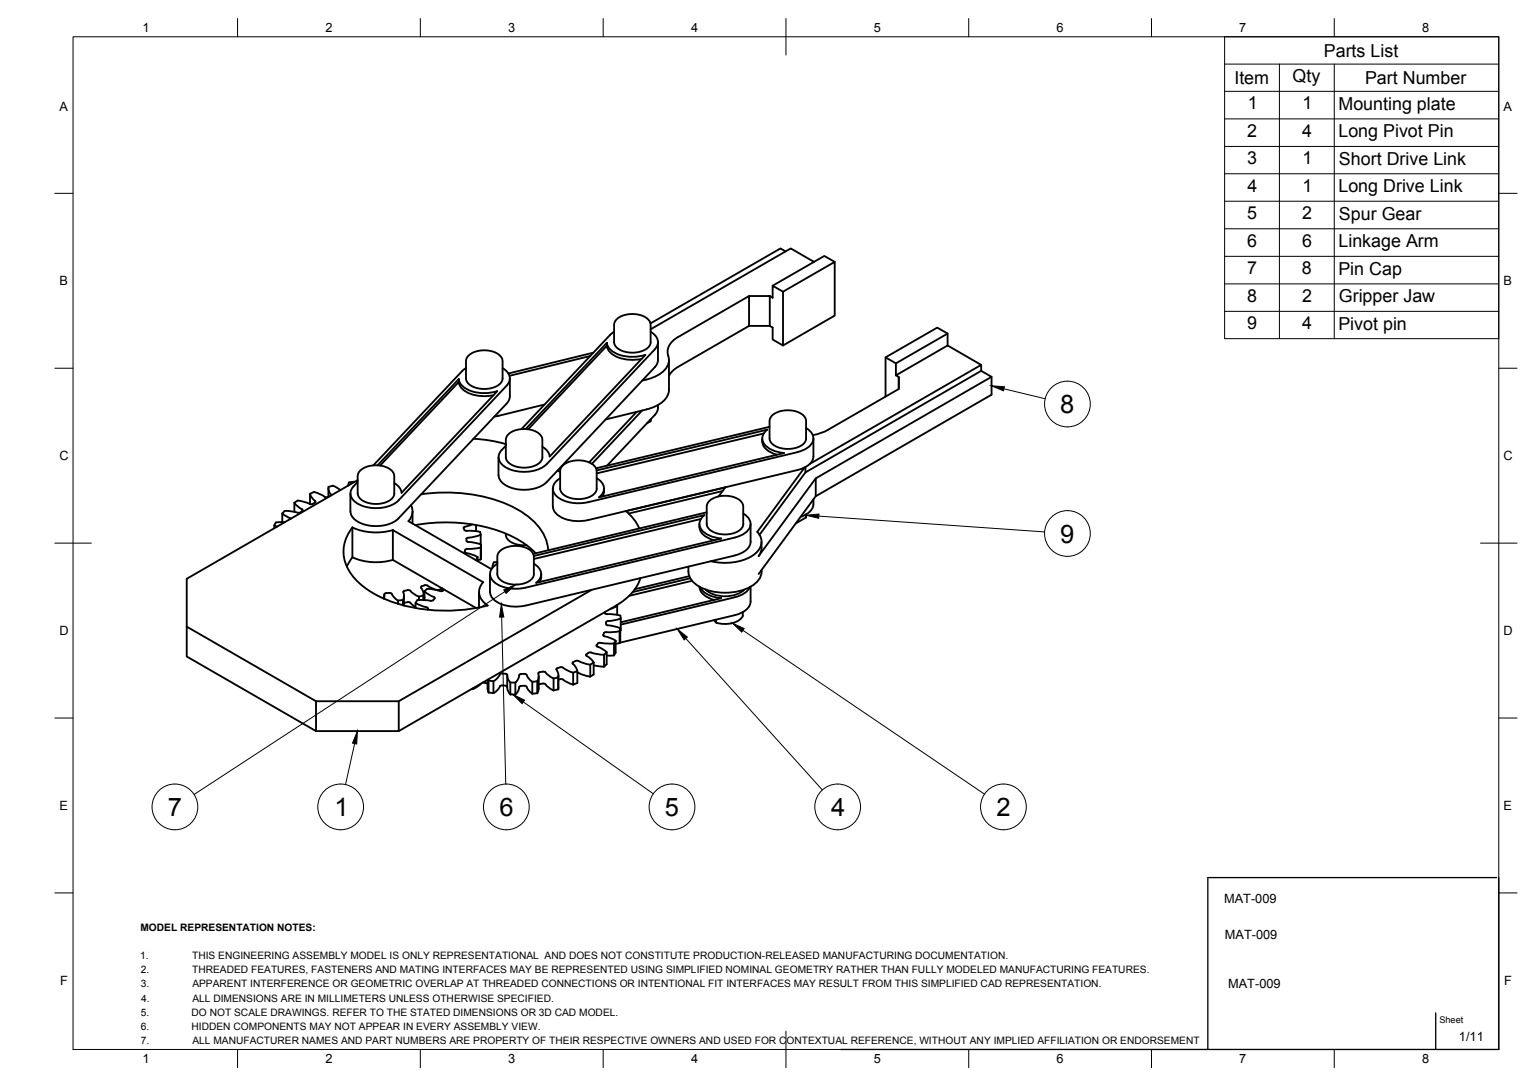
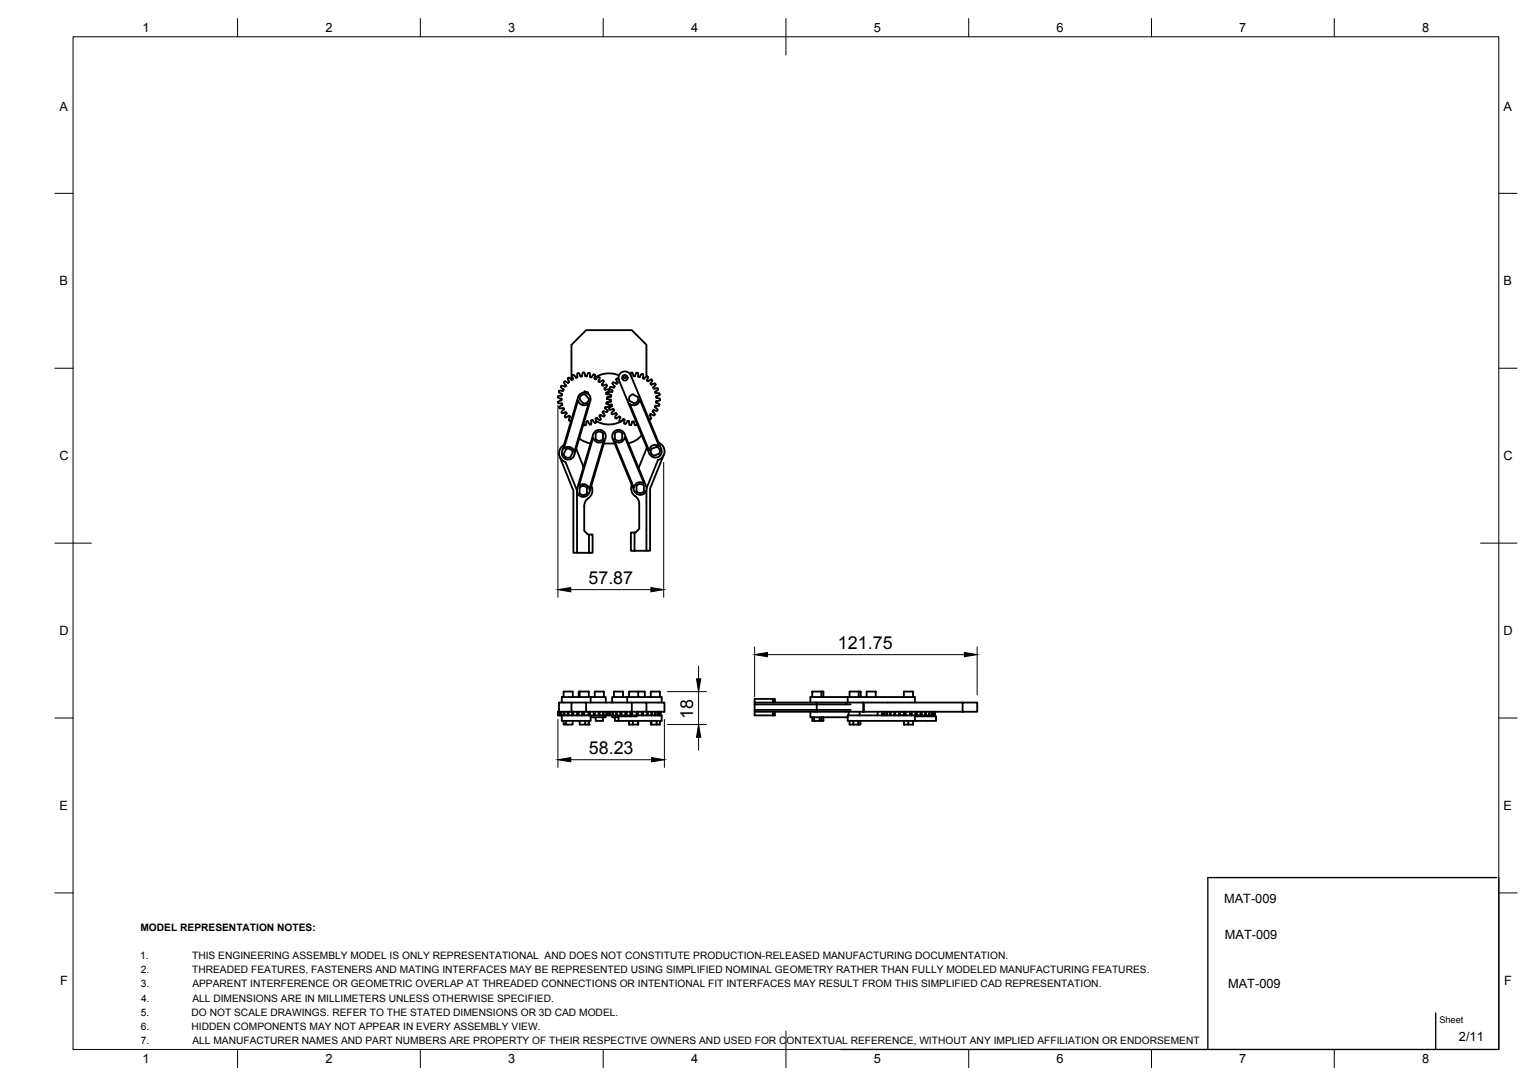
ISO-10303-21;
HEADER;
/* Generated by software containing ST-Developer
 * from STEP Tools, Inc. (www.steptools.com) 
 */

FILE_DESCRIPTION(
/* description */ ('STEP AP214'),
/* implementation_level */ '2;1');

FILE_NAME(
/* name */ 'MAT-009.step',
/* time_stamp */ '2026-11-14T05:43:09-08:00',
/* author */ (''),
/* organization */ (''),
/* preprocessor_version */ 'ST-DEVELOPER v20.2',
/* originating_system */ 'Autodesk Translation Framework v15.17.0.0',
/* authorisation */ '');

FILE_SCHEMA (('AUTOMOTIVE_DESIGN { 1 0 10303 214 3 1 1 }'));
ENDSEC;

DATA;
#10=MECHANICAL_DESIGN_GEOMETRIC_PRESENTATION_REPRESENTATION('',(#146,#147,
#148,#149,#150,#151,#152,#153,#154),#11933);
#11=ITEM_DEFINED_TRANSFORMATION($,$,#6753,#7621);
#12=ITEM_DEFINED_TRANSFORMATION($,$,#7486,#7622);
#13=ITEM_DEFINED_TRANSFORMATION($,$,#6800,#7623);
#14=ITEM_DEFINED_TRANSFORMATION($,$,#6849,#7624);
#15=ITEM_DEFINED_TRANSFORMATION($,$,#6899,#7625);
#16=ITEM_DEFINED_TRANSFORMATION($,$,#7521,#7626);
#17=ITEM_DEFINED_TRANSFORMATION($,$,#7591,#7627);
#18=ITEM_DEFINED_TRANSFORMATION($,$,#7448,#7628);
#19=ITEM_DEFINED_TRANSFORMATION($,$,#7556,#7629);
#20=ITEM_DEFINED_TRANSFORMATION($,$,#7486,#7630);
#21=ITEM_DEFINED_TRANSFORMATION($,$,#6899,#7631);
#22=ITEM_DEFINED_TRANSFORMATION($,$,#7521,#7632);
#23=ITEM_DEFINED_TRANSFORMATION($,$,#7591,#7633);
#24=ITEM_DEFINED_TRANSFORMATION($,$,#7448,#7634);
#25=ITEM_DEFINED_TRANSFORMATION($,$,#7486,#7635);
#26=ITEM_DEFINED_TRANSFORMATION($,$,#7486,#7636);
#27=ITEM_DEFINED_TRANSFORMATION($,$,#7591,#7637);
#28=ITEM_DEFINED_TRANSFORMATION($,$,#7591,#7638);
#29=ITEM_DEFINED_TRANSFORMATION($,$,#7521,#7639);
#30=ITEM_DEFINED_TRANSFORMATION($,$,#7521,#7640);
#31=ITEM_DEFINED_TRANSFORMATION($,$,#7521,#7641);
#32=ITEM_DEFINED_TRANSFORMATION($,$,#7521,#7642);
#33=ITEM_DEFINED_TRANSFORMATION($,$,#7556,#7643);
#34=ITEM_DEFINED_TRANSFORMATION($,$,#7556,#7644);
#35=ITEM_DEFINED_TRANSFORMATION($,$,#7556,#7645);
#36=ITEM_DEFINED_TRANSFORMATION($,$,#7591,#7646);
#37=ITEM_DEFINED_TRANSFORMATION($,$,#7591,#7647);
#38=ITEM_DEFINED_TRANSFORMATION($,$,#7591,#7648);
#39=ITEM_DEFINED_TRANSFORMATION($,$,#7591,#7649);
#40=(
REPRESENTATION_RELATIONSHIP($,$,#11988,#11987)
REPRESENTATION_RELATIONSHIP_WITH_TRANSFORMATION(#11)
SHAPE_REPRESENTATION_RELATIONSHIP()
);
#41=(
REPRESENTATION_RELATIONSHIP($,$,#11993,#11987)
REPRESENTATION_RELATIONSHIP_WITH_TRANSFORMATION(#12)
SHAPE_REPRESENTATION_RELATIONSHIP()
);
#42=(
REPRESENTATION_RELATIONSHIP($,$,#11989,#11987)
REPRESENTATION_RELATIONSHIP_WITH_TRANSFORMATION(#13)
SHAPE_REPRESENTATION_RELATIONSHIP()
);
#43=(
REPRESENTATION_RELATIONSHIP($,$,#11990,#11987)
REPRESENTATION_RELATIONSHIP_WITH_TRANSFORMATION(#14)
SHAPE_REPRESENTATION_RELATIONSHIP()
);
#44=(
REPRESENTATION_RELATIONSHIP($,$,#11991,#11987)
REPRESENTATION_RELATIONSHIP_WITH_TRANSFORMATION(#15)
SHAPE_REPRESENTATION_RELATIONSHIP()
);
#45=(
REPRESENTATION_RELATIONSHIP($,$,#11994,#11987)
REPRESENTATION_RELATIONSHIP_WITH_TRANSFORMATION(#16)
SHAPE_REPRESENTATION_RELATIONSHIP()
);
#46=(
REPRESENTATION_RELATIONSHIP($,$,#11996,#11987)
REPRESENTATION_RELATIONSHIP_WITH_TRANSFORMATION(#17)
SHAPE_REPRESENTATION_RELATIONSHIP()
);
#47=(
REPRESENTATION_RELATIONSHIP($,$,#11992,#11987)
REPRESENTATION_RELATIONSHIP_WITH_TRANSFORMATION(#18)
SHAPE_REPRESENTATION_RELATIONSHIP()
);
#48=(
REPRESENTATION_RELATIONSHIP($,$,#11995,#11987)
REPRESENTATION_RELATIONSHIP_WITH_TRANSFORMATION(#19)
SHAPE_REPRESENTATION_RELATIONSHIP()
);
#49=(
REPRESENTATION_RELATIONSHIP($,$,#11993,#11987)
REPRESENTATION_RELATIONSHIP_WITH_TRANSFORMATION(#20)
SHAPE_REPRESENTATION_RELATIONSHIP()
);
#50=(
REPRESENTATION_RELATIONSHIP($,$,#11991,#11987)
REPRESENTATION_RELATIONSHIP_WITH_TRANSFORMATION(#21)
SHAPE_REPRESENTATION_RELATIONSHIP()
);
#51=(
REPRESENTATION_RELATIONSHIP($,$,#11994,#11987)
REPRESENTATION_RELATIONSHIP_WITH_TRANSFORMATION(#22)
SHAPE_REPRESENTATION_RELATIONSHIP()
);
#52=(
REPRESENTATION_RELATIONSHIP($,$,#11996,#11987)
REPRESENTATION_RELATIONSHIP_WITH_TRANSFORMATION(#23)
SHAPE_REPRESENTATION_RELATIONSHIP()
);
#53=(
REPRESENTATION_RELATIONSHIP($,$,#11992,#11987)
REPRESENTATION_RELATIONSHIP_WITH_TRANSFORMATION(#24)
SHAPE_REPRESENTATION_RELATIONSHIP()
);
#54=(
REPRESENTATION_RELATIONSHIP($,$,#11993,#11987)
REPRESENTATION_RELATIONSHIP_WITH_TRANSFORMATION(#25)
SHAPE_REPRESENTATION_RELATIONSHIP()
);
#55=(
REPRESENTATION_RELATIONSHIP($,$,#11993,#11987)
REPRESENTATION_RELATIONSHIP_WITH_TRANSFORMATION(#26)
SHAPE_REPRESENTATION_RELATIONSHIP()
);
#56=(
REPRESENTATION_RELATIONSHIP($,$,#11996,#11987)
REPRESENTATION_RELATIONSHIP_WITH_TRANSFORMATION(#27)
SHAPE_REPRESENTATION_RELATIONSHIP()
);
#57=(
REPRESENTATION_RELATIONSHIP($,$,#11996,#11987)
REPRESENTATION_RELATIONSHIP_WITH_TRANSFORMATION(#28)
SHAPE_REPRESENTATION_RELATIONSHIP()
);
#58=(
REPRESENTATION_RELATIONSHIP($,$,#11994,#11987)
REPRESENTATION_RELATIONSHIP_WITH_TRANSFORMATION(#29)
SHAPE_REPRESENTATION_RELATIONSHIP()
);
#59=(
REPRESENTATION_RELATIONSHIP($,$,#11994,#11987)
REPRESENTATION_RELATIONSHIP_WITH_TRANSFORMATION(#30)
SHAPE_REPRESENTATION_RELATIONSHIP()
);
#60=(
REPRESENTATION_RELATIONSHIP($,$,#11994,#11987)
REPRESENTATION_RELATIONSHIP_WITH_TRANSFORMATION(#31)
SHAPE_REPRESENTATION_RELATIONSHIP()
);
#61=(
REPRESENTATION_RELATIONSHIP($,$,#11994,#11987)
REPRESENTATION_RELATIONSHIP_WITH_TRANSFORMATION(#32)
SHAPE_REPRESENTATION_RELATIONSHIP()
);
#62=(
REPRESENTATION_RELATIONSHIP($,$,#11995,#11987)
REPRESENTATION_RELATIONSHIP_WITH_TRANSFORMATION(#33)
SHAPE_REPRESENTATION_RELATIONSHIP()
);
#63=(
REPRESENTATION_RELATIONSHIP($,$,#11995,#11987)
REPRESENTATION_RELATIONSHIP_WITH_TRANSFORMATION(#34)
SHAPE_REPRESENTATION_RELATIONSHIP()
);
#64=(
REPRESENTATION_RELATIONSHIP($,$,#11995,#11987)
REPRESENTATION_RELATIONSHIP_WITH_TRANSFORMATION(#35)
SHAPE_REPRESENTATION_RELATIONSHIP()
);
#65=(
REPRESENTATION_RELATIONSHIP($,$,#11996,#11987)
REPRESENTATION_RELATIONSHIP_WITH_TRANSFORMATION(#36)
SHAPE_REPRESENTATION_RELATIONSHIP()
);
#66=(
REPRESENTATION_RELATIONSHIP($,$,#11996,#11987)
REPRESENTATION_RELATIONSHIP_WITH_TRANSFORMATION(#37)
SHAPE_REPRESENTATION_RELATIONSHIP()
);
#67=(
REPRESENTATION_RELATIONSHIP($,$,#11996,#11987)
REPRESENTATION_RELATIONSHIP_WITH_TRANSFORMATION(#38)
SHAPE_REPRESENTATION_RELATIONSHIP()
);
#68=(
REPRESENTATION_RELATIONSHIP($,$,#11996,#11987)
REPRESENTATION_RELATIONSHIP_WITH_TRANSFORMATION(#39)
SHAPE_REPRESENTATION_RELATIONSHIP()
);
#69=CONTEXT_DEPENDENT_SHAPE_REPRESENTATION(#40,#11958);
#70=CONTEXT_DEPENDENT_SHAPE_REPRESENTATION(#41,#11959);
#71=CONTEXT_DEPENDENT_SHAPE_REPRESENTATION(#42,#11960);
#72=CONTEXT_DEPENDENT_SHAPE_REPRESENTATION(#43,#11961);
#73=CONTEXT_DEPENDENT_SHAPE_REPRESENTATION(#44,#11962);
#74=CONTEXT_DEPENDENT_SHAPE_REPRESENTATION(#45,#11963);
#75=CONTEXT_DEPENDENT_SHAPE_REPRESENTATION(#46,#11964);
#76=CONTEXT_DEPENDENT_SHAPE_REPRESENTATION(#47,#11965);
#77=CONTEXT_DEPENDENT_SHAPE_REPRESENTATION(#48,#11966);
#78=CONTEXT_DEPENDENT_SHAPE_REPRESENTATION(#49,#11967);
#79=CONTEXT_DEPENDENT_SHAPE_REPRESENTATION(#50,#11968);
#80=CONTEXT_DEPENDENT_SHAPE_REPRESENTATION(#51,#11969);
#81=CONTEXT_DEPENDENT_SHAPE_REPRESENTATION(#52,#11970);
#82=CONTEXT_DEPENDENT_SHAPE_REPRESENTATION(#53,#11971);
#83=CONTEXT_DEPENDENT_SHAPE_REPRESENTATION(#54,#11972);
#84=CONTEXT_DEPENDENT_SHAPE_REPRESENTATION(#55,#11973);
#85=CONTEXT_DEPENDENT_SHAPE_REPRESENTATION(#56,#11974);
#86=CONTEXT_DEPENDENT_SHAPE_REPRESENTATION(#57,#11975);
#87=CONTEXT_DEPENDENT_SHAPE_REPRESENTATION(#58,#11976);
#88=CONTEXT_DEPENDENT_SHAPE_REPRESENTATION(#59,#11977);
#89=CONTEXT_DEPENDENT_SHAPE_REPRESENTATION(#60,#11978);
#90=CONTEXT_DEPENDENT_SHAPE_REPRESENTATION(#61,#11979);
#91=CONTEXT_DEPENDENT_SHAPE_REPRESENTATION(#62,#11980);
#92=CONTEXT_DEPENDENT_SHAPE_REPRESENTATION(#63,#11981);
#93=CONTEXT_DEPENDENT_SHAPE_REPRESENTATION(#64,#11982);
#94=CONTEXT_DEPENDENT_SHAPE_REPRESENTATION(#65,#11983);
#95=CONTEXT_DEPENDENT_SHAPE_REPRESENTATION(#66,#11984);
#96=CONTEXT_DEPENDENT_SHAPE_REPRESENTATION(#67,#11985);
#97=CONTEXT_DEPENDENT_SHAPE_REPRESENTATION(#68,#11986);
#98=NEXT_ASSEMBLY_USAGE_OCCURRENCE('Mounting Plate:1',
'Mounting Plate:1','Mounting Plate:1',#11998,#11999,'Mounting Plate:1');
#99=NEXT_ASSEMBLY_USAGE_OCCURRENCE('Long Pivot Pin:1',
'Long Pivot Pin:1','Long Pivot Pin:1',#11998,#12004,'Long Pivot Pin:1');
#100=NEXT_ASSEMBLY_USAGE_OCCURRENCE('Short Drive Link:1',
'Short Drive Link:1','Short Drive Link:1',#11998,#12000,
'Short Drive Link:1');
#101=NEXT_ASSEMBLY_USAGE_OCCURRENCE('Long Drive Link:1',
'Long Drive Link:1','Long Drive Link:1',#11998,#12001,
'Long Drive Link:1');
#102=NEXT_ASSEMBLY_USAGE_OCCURRENCE('Spur Gear:1','Spur Gear:1',
'Spur Gear:1',#11998,#12002,'Spur Gear:1');
#103=NEXT_ASSEMBLY_USAGE_OCCURRENCE('Linkage Arm:1','Linkage Arm:1',
'Linkage Arm:1',#11998,#12005,'Linkage Arm:1');
#104=NEXT_ASSEMBLY_USAGE_OCCURRENCE('Pin Cap:1','Pin Cap:1','Pin Cap:1',
#11998,#12007,'Pin Cap:1');
#105=NEXT_ASSEMBLY_USAGE_OCCURRENCE('Gripper Jaw:1','Gripper Jaw:1',
'Gripper Jaw:1',#11998,#12003,'Gripper Jaw:1');
#106=NEXT_ASSEMBLY_USAGE_OCCURRENCE('Pivot Pin:1','Pivot Pin:1',
'Pivot Pin:1',#11998,#12006,'Pivot Pin:1');
#107=NEXT_ASSEMBLY_USAGE_OCCURRENCE('Long Pivot Pin:2',
'Long Pivot Pin:2','Long Pivot Pin:2',#11998,#12004,'Long Pivot Pin:2');
#108=NEXT_ASSEMBLY_USAGE_OCCURRENCE('Spur Gear:2','Spur Gear:2',
'Spur Gear:2',#11998,#12002,'Spur Gear:2');
#109=NEXT_ASSEMBLY_USAGE_OCCURRENCE('Linkage Arm:2','Linkage Arm:2',
'Linkage Arm:2',#11998,#12005,'Linkage Arm:2');
#110=NEXT_ASSEMBLY_USAGE_OCCURRENCE('Pin Cap:2','Pin Cap:2','Pin Cap:2',
#11998,#12007,'Pin Cap:2');
#111=NEXT_ASSEMBLY_USAGE_OCCURRENCE('Gripper Jaw:2','Gripper Jaw:2',
'Gripper Jaw:2',#11998,#12003,'Gripper Jaw:2');
#112=NEXT_ASSEMBLY_USAGE_OCCURRENCE('Long Pivot Pin:3',
'Long Pivot Pin:3','Long Pivot Pin:3',#11998,#12004,'Long Pivot Pin:3');
#113=NEXT_ASSEMBLY_USAGE_OCCURRENCE('Long Pivot Pin:4',
'Long Pivot Pin:4','Long Pivot Pin:4',#11998,#12004,'Long Pivot Pin:4');
#114=NEXT_ASSEMBLY_USAGE_OCCURRENCE('Pin Cap:3','Pin Cap:3','Pin Cap:3',
#11998,#12007,'Pin Cap:3');
#115=NEXT_ASSEMBLY_USAGE_OCCURRENCE('Pin Cap:4','Pin Cap:4','Pin Cap:4',
#11998,#12007,'Pin Cap:4');
#116=NEXT_ASSEMBLY_USAGE_OCCURRENCE('Linkage Arm:3','Linkage Arm:3',
'Linkage Arm:3',#11998,#12005,'Linkage Arm:3');
#117=NEXT_ASSEMBLY_USAGE_OCCURRENCE('Linkage Arm:4','Linkage Arm:4',
'Linkage Arm:4',#11998,#12005,'Linkage Arm:4');
#118=NEXT_ASSEMBLY_USAGE_OCCURRENCE('Linkage Arm:5','Linkage Arm:5',
'Linkage Arm:5',#11998,#12005,'Linkage Arm:5');
#119=NEXT_ASSEMBLY_USAGE_OCCURRENCE('Linkage Arm:6','Linkage Arm:6',
'Linkage Arm:6',#11998,#12005,'Linkage Arm:6');
#120=NEXT_ASSEMBLY_USAGE_OCCURRENCE('Pivot Pin:2','Pivot Pin:2',
'Pivot Pin:2',#11998,#12006,'Pivot Pin:2');
#121=NEXT_ASSEMBLY_USAGE_OCCURRENCE('Pivot Pin:3','Pivot Pin:3',
'Pivot Pin:3',#11998,#12006,'Pivot Pin:3');
#122=NEXT_ASSEMBLY_USAGE_OCCURRENCE('Pivot Pin:4','Pivot Pin:4',
'Pivot Pin:4',#11998,#12006,'Pivot Pin:4');
#123=NEXT_ASSEMBLY_USAGE_OCCURRENCE('Pin Cap:5','Pin Cap:5','Pin Cap:5',
#11998,#12007,'Pin Cap:5');
#124=NEXT_ASSEMBLY_USAGE_OCCURRENCE('Pin Cap:6','Pin Cap:6','Pin Cap:6',
#11998,#12007,'Pin Cap:6');
#125=NEXT_ASSEMBLY_USAGE_OCCURRENCE('Pin Cap:7','Pin Cap:7','Pin Cap:7',
#11998,#12007,'Pin Cap:7');
#126=NEXT_ASSEMBLY_USAGE_OCCURRENCE('Pin Cap:8','Pin Cap:8','Pin Cap:8',
#11998,#12007,'Pin Cap:8');
#127=TOROIDAL_SURFACE('',#7592,2.4,0.1);
#128=SHAPE_REPRESENTATION_RELATIONSHIP('SRR','None',#11988,#137);
#129=SHAPE_REPRESENTATION_RELATIONSHIP('SRR','None',#11989,#138);
#130=SHAPE_REPRESENTATION_RELATIONSHIP('SRR','None',#11990,#139);
#131=SHAPE_REPRESENTATION_RELATIONSHIP('SRR','None',#11991,#140);
#132=SHAPE_REPRESENTATION_RELATIONSHIP('SRR','None',#11992,#141);
#133=SHAPE_REPRESENTATION_RELATIONSHIP('SRR','None',#11993,#142);
#134=SHAPE_REPRESENTATION_RELATIONSHIP('SRR','None',#11994,#143);
#135=SHAPE_REPRESENTATION_RELATIONSHIP('SRR','None',#11995,#144);
#136=SHAPE_REPRESENTATION_RELATIONSHIP('SRR','None',#11996,#145);
#137=ADVANCED_BREP_SHAPE_REPRESENTATION('',(#155),#11924);
#138=ADVANCED_BREP_SHAPE_REPRESENTATION('',(#156),#11925);
#139=ADVANCED_BREP_SHAPE_REPRESENTATION('',(#157),#11926);
#140=ADVANCED_BREP_SHAPE_REPRESENTATION('',(#158),#11927);
#141=ADVANCED_BREP_SHAPE_REPRESENTATION('',(#159),#11928);
#142=ADVANCED_BREP_SHAPE_REPRESENTATION('',(#160),#11929);
#143=ADVANCED_BREP_SHAPE_REPRESENTATION('',(#161),#11930);
#144=ADVANCED_BREP_SHAPE_REPRESENTATION('',(#162),#11931);
#145=ADVANCED_BREP_SHAPE_REPRESENTATION('',(#163),#11932);
#146=STYLED_ITEM('',(#12042),#155);
#147=STYLED_ITEM('',(#12042),#156);
#148=STYLED_ITEM('',(#12043),#157);
#149=STYLED_ITEM('',(#12043),#158);
#150=STYLED_ITEM('',(#12043),#159);
#151=STYLED_ITEM('',(#12042),#160);
#152=STYLED_ITEM('',(#12044),#161);
#153=STYLED_ITEM('',(#12043),#162);
#154=STYLED_ITEM('',(#12043),#163);
#155=MANIFOLD_SOLID_BREP('Body1',#6643);
#156=MANIFOLD_SOLID_BREP('Body1',#6644);
#157=MANIFOLD_SOLID_BREP('Body1',#6645);
#158=MANIFOLD_SOLID_BREP('Body1',#6646);
#159=MANIFOLD_SOLID_BREP('Body1',#6647);
#160=MANIFOLD_SOLID_BREP('Body1',#6648);
#161=MANIFOLD_SOLID_BREP('Body1',#6649);
#162=MANIFOLD_SOLID_BREP('Body1',#6650);
#163=MANIFOLD_SOLID_BREP('Body1',#6651);
#164=FACE_BOUND('',#692,.T.);
#165=FACE_BOUND('',#693,.T.);
#166=FACE_BOUND('',#694,.T.);
#167=FACE_BOUND('',#695,.T.);
#168=FACE_BOUND('',#696,.T.);
#169=FACE_BOUND('',#697,.T.);
#170=FACE_BOUND('',#699,.T.);
#171=FACE_BOUND('',#700,.T.);
#172=FACE_BOUND('',#701,.T.);
#173=FACE_BOUND('',#702,.T.);
#174=FACE_BOUND('',#703,.T.);
#175=FACE_BOUND('',#704,.T.);
#176=FACE_BOUND('',#714,.T.);
#177=FACE_BOUND('',#715,.T.);
#178=FACE_BOUND('',#717,.T.);
#179=FACE_BOUND('',#718,.T.);
#180=FACE_BOUND('',#719,.T.);
#181=FACE_BOUND('',#737,.T.);
#182=FACE_BOUND('',#739,.T.);
#183=FACE_BOUND('',#748,.T.);
#184=FACE_BOUND('',#750,.T.);
#185=FACE_BOUND('',#751,.T.);
#186=FACE_BOUND('',#753,.T.);
#187=FACE_BOUND('',#754,.T.);
#188=FACE_BOUND('',#755,.T.);
#189=FACE_BOUND('',#756,.T.);
#190=FACE_BOUND('',#773,.T.);
#191=FACE_BOUND('',#775,.T.);
#192=FACE_BOUND('',#825,.T.);
#193=FACE_BOUND('',#827,.T.);
#194=FACE_BOUND('',#968,.T.);
#195=FACE_BOUND('',#969,.T.);
#196=FACE_BOUND('',#972,.T.);
#197=FACE_BOUND('',#973,.T.);
#198=FACE_BOUND('',#998,.T.);
#199=FACE_BOUND('',#1000,.T.);
#200=FACE_BOUND('',#1019,.T.);
#201=FACE_BOUND('',#1020,.T.);
#202=FACE_BOUND('',#1021,.T.);
#203=FACE_BOUND('',#1026,.T.);
#204=FACE_BOUND('',#1027,.T.);
#205=FACE_BOUND('',#1028,.T.);
#206=FACE_BOUND('',#1042,.T.);
#207=FACE_BOUND('',#1051,.T.);
#208=FACE_BOUND('',#1064,.T.);
#209=PLANE('',#6766);
#210=PLANE('',#6767);
#211=PLANE('',#6768);
#212=PLANE('',#6769);
#213=PLANE('',#6770);
#214=PLANE('',#6777);
#215=PLANE('',#6787);
#216=PLANE('',#6791);
#217=PLANE('',#6792);
#218=PLANE('',#6795);
#219=PLANE('',#6821);
#220=PLANE('',#6825);
#221=PLANE('',#6828);
#222=PLANE('',#6830);
#223=PLANE('',#6833);
#224=PLANE('',#6834);
#225=PLANE('',#6835);
#226=PLANE('',#6836);
#227=PLANE('',#6839);
#228=PLANE('',#6840);
#229=PLANE('',#6841);
#230=PLANE('',#6842);
#231=PLANE('',#6845);
#232=PLANE('',#6846);
#233=PLANE('',#6847);
#234=PLANE('',#6848);
#235=PLANE('',#6871);
#236=PLANE('',#6872);
#237=PLANE('',#6876);
#238=PLANE('',#6879);
#239=PLANE('',#6881);
#240=PLANE('',#6884);
#241=PLANE('',#6885);
#242=PLANE('',#6886);
#243=PLANE('',#6887);
#244=PLANE('',#6890);
#245=PLANE('',#6891);
#246=PLANE('',#6892);
#247=PLANE('',#6895);
#248=PLANE('',#6896);
#249=PLANE('',#6897);
#250=PLANE('',#6898);
#251=PLANE('',#7044);
#252=PLANE('',#7178);
#253=PLANE('',#7445);
#254=PLANE('',#7446);
#255=PLANE('',#7447);
#256=PLANE('',#7460);
#257=PLANE('',#7463);
#258=PLANE('',#7464);
#259=PLANE('',#7467);
#260=PLANE('',#7468);
#261=PLANE('',#7469);
#262=PLANE('',#7470);
#263=PLANE('',#7471);
#264=PLANE('',#7473);
#265=PLANE('',#7474);
#266=PLANE('',#7475);
#267=PLANE('',#7476);
#268=PLANE('',#7477);
#269=PLANE('',#7478);
#270=PLANE('',#7479);
#271=PLANE('',#7480);
#272=PLANE('',#7481);
#273=PLANE('',#7482);
#274=PLANE('',#7483);
#275=PLANE('',#7484);
#276=PLANE('',#7497);
#277=PLANE('',#7501);
#278=PLANE('',#7502);
#279=PLANE('',#7507);
#280=PLANE('',#7510);
#281=PLANE('',#7511);
#282=PLANE('',#7512);
#283=PLANE('',#7516);
#284=PLANE('',#7517);
#285=PLANE('',#7518);
#286=PLANE('',#7519);
#287=PLANE('',#7520);
#288=PLANE('',#7537);
#289=PLANE('',#7540);
#290=PLANE('',#7541);
#291=PLANE('',#7544);
#292=PLANE('',#7546);
#293=PLANE('',#7549);
#294=PLANE('',#7550);
#295=PLANE('',#7553);
#296=PLANE('',#7554);
#297=PLANE('',#7555);
#298=PLANE('',#7567);
#299=PLANE('',#7571);
#300=PLANE('',#7572);
#301=PLANE('',#7576);
#302=PLANE('',#7577);
#303=PLANE('',#7578);
#304=PLANE('',#7579);
#305=PLANE('',#7580);
#306=PLANE('',#7581);
#307=PLANE('',#7586);
#308=PLANE('',#7589);
#309=PLANE('',#7590);
#310=PLANE('',#7609);
#311=PLANE('',#7611);
#312=PLANE('',#7612);
#313=PLANE('',#7615);
#314=PLANE('',#7616);
#315=PLANE('',#7617);
#316=PLANE('',#7618);
#317=PLANE('',#7619);
#318=PLANE('',#7620);
#319=FACE_OUTER_BOUND('',#673,.T.);
#320=FACE_OUTER_BOUND('',#674,.T.);
#321=FACE_OUTER_BOUND('',#675,.T.);
#322=FACE_OUTER_BOUND('',#676,.T.);
#323=FACE_OUTER_BOUND('',#677,.T.);
#324=FACE_OUTER_BOUND('',#678,.T.);
#325=FACE_OUTER_BOUND('',#679,.T.);
#326=FACE_OUTER_BOUND('',#680,.T.);
#327=FACE_OUTER_BOUND('',#681,.T.);
#328=FACE_OUTER_BOUND('',#682,.T.);
#329=FACE_OUTER_BOUND('',#683,.T.);
#330=FACE_OUTER_BOUND('',#684,.T.);
#331=FACE_OUTER_BOUND('',#685,.T.);
#332=FACE_OUTER_BOUND('',#686,.T.);
#333=FACE_OUTER_BOUND('',#687,.T.);
#334=FACE_OUTER_BOUND('',#688,.T.);
#335=FACE_OUTER_BOUND('',#689,.T.);
#336=FACE_OUTER_BOUND('',#690,.T.);
#337=FACE_OUTER_BOUND('',#691,.T.);
#338=FACE_OUTER_BOUND('',#698,.T.);
#339=FACE_OUTER_BOUND('',#705,.T.);
#340=FACE_OUTER_BOUND('',#706,.T.);
#341=FACE_OUTER_BOUND('',#707,.T.);
#342=FACE_OUTER_BOUND('',#708,.T.);
#343=FACE_OUTER_BOUND('',#709,.T.);
#344=FACE_OUTER_BOUND('',#710,.T.);
#345=FACE_OUTER_BOUND('',#711,.T.);
#346=FACE_OUTER_BOUND('',#712,.T.);
#347=FACE_OUTER_BOUND('',#713,.T.);
#348=FACE_OUTER_BOUND('',#716,.T.);
#349=FACE_OUTER_BOUND('',#720,.T.);
#350=FACE_OUTER_BOUND('',#721,.T.);
#351=FACE_OUTER_BOUND('',#722,.T.);
#352=FACE_OUTER_BOUND('',#723,.T.);
#353=FACE_OUTER_BOUND('',#724,.T.);
#354=FACE_OUTER_BOUND('',#725,.T.);
#355=FACE_OUTER_BOUND('',#726,.T.);
#356=FACE_OUTER_BOUND('',#727,.T.);
#357=FACE_OUTER_BOUND('',#728,.T.);
#358=FACE_OUTER_BOUND('',#729,.T.);
#359=FACE_OUTER_BOUND('',#730,.T.);
#360=FACE_OUTER_BOUND('',#731,.T.);
#361=FACE_OUTER_BOUND('',#732,.T.);
#362=FACE_OUTER_BOUND('',#733,.T.);
#363=FACE_OUTER_BOUND('',#734,.T.);
#364=FACE_OUTER_BOUND('',#735,.T.);
#365=FACE_OUTER_BOUND('',#736,.T.);
#366=FACE_OUTER_BOUND('',#738,.T.);
#367=FACE_OUTER_BOUND('',#740,.T.);
#368=FACE_OUTER_BOUND('',#741,.T.);
#369=FACE_OUTER_BOUND('',#742,.T.);
#370=FACE_OUTER_BOUND('',#743,.T.);
#371=FACE_OUTER_BOUND('',#744,.T.);
#372=FACE_OUTER_BOUND('',#745,.T.);
#373=FACE_OUTER_BOUND('',#746,.T.);
#374=FACE_OUTER_BOUND('',#747,.T.);
#375=FACE_OUTER_BOUND('',#749,.T.);
#376=FACE_OUTER_BOUND('',#752,.T.);
#377=FACE_OUTER_BOUND('',#757,.T.);
#378=FACE_OUTER_BOUND('',#758,.T.);
#379=FACE_OUTER_BOUND('',#759,.T.);
#380=FACE_OUTER_BOUND('',#760,.T.);
#381=FACE_OUTER_BOUND('',#761,.T.);
#382=FACE_OUTER_BOUND('',#762,.T.);
#383=FACE_OUTER_BOUND('',#763,.T.);
#384=FACE_OUTER_BOUND('',#764,.T.);
#385=FACE_OUTER_BOUND('',#765,.T.);
#386=FACE_OUTER_BOUND('',#766,.T.);
#387=FACE_OUTER_BOUND('',#767,.T.);
#388=FACE_OUTER_BOUND('',#768,.T.);
#389=FACE_OUTER_BOUND('',#769,.T.);
#390=FACE_OUTER_BOUND('',#770,.T.);
#391=FACE_OUTER_BOUND('',#771,.T.);
#392=FACE_OUTER_BOUND('',#772,.T.);
#393=FACE_OUTER_BOUND('',#774,.T.);
#394=FACE_OUTER_BOUND('',#776,.T.);
#395=FACE_OUTER_BOUND('',#777,.T.);
#396=FACE_OUTER_BOUND('',#778,.T.);
#397=FACE_OUTER_BOUND('',#779,.T.);
#398=FACE_OUTER_BOUND('',#780,.T.);
#399=FACE_OUTER_BOUND('',#781,.T.);
#400=FACE_OUTER_BOUND('',#782,.T.);
#401=FACE_OUTER_BOUND('',#783,.T.);
#402=FACE_OUTER_BOUND('',#784,.T.);
#403=FACE_OUTER_BOUND('',#785,.T.);
#404=FACE_OUTER_BOUND('',#786,.T.);
#405=FACE_OUTER_BOUND('',#787,.T.);
#406=FACE_OUTER_BOUND('',#788,.T.);
#407=FACE_OUTER_BOUND('',#789,.T.);
#408=FACE_OUTER_BOUND('',#790,.T.);
#409=FACE_OUTER_BOUND('',#791,.T.);
#410=FACE_OUTER_BOUND('',#792,.T.);
#411=FACE_OUTER_BOUND('',#793,.T.);
#412=FACE_OUTER_BOUND('',#794,.T.);
#413=FACE_OUTER_BOUND('',#795,.T.);
#414=FACE_OUTER_BOUND('',#796,.T.);
#415=FACE_OUTER_BOUND('',#797,.T.);
#416=FACE_OUTER_BOUND('',#798,.T.);
#417=FACE_OUTER_BOUND('',#799,.T.);
#418=FACE_OUTER_BOUND('',#800,.T.);
#419=FACE_OUTER_BOUND('',#801,.T.);
#420=FACE_OUTER_BOUND('',#802,.T.);
#421=FACE_OUTER_BOUND('',#803,.T.);
#422=FACE_OUTER_BOUND('',#804,.T.);
#423=FACE_OUTER_BOUND('',#805,.T.);
#424=FACE_OUTER_BOUND('',#806,.T.);
#425=FACE_OUTER_BOUND('',#807,.T.);
#426=FACE_OUTER_BOUND('',#808,.T.);
#427=FACE_OUTER_BOUND('',#809,.T.);
#428=FACE_OUTER_BOUND('',#810,.T.);
#429=FACE_OUTER_BOUND('',#811,.T.);
#430=FACE_OUTER_BOUND('',#812,.T.);
#431=FACE_OUTER_BOUND('',#813,.T.);
#432=FACE_OUTER_BOUND('',#814,.T.);
#433=FACE_OUTER_BOUND('',#815,.T.);
#434=FACE_OUTER_BOUND('',#816,.T.);
#435=FACE_OUTER_BOUND('',#817,.T.);
#436=FACE_OUTER_BOUND('',#818,.T.);
#437=FACE_OUTER_BOUND('',#819,.T.);
#438=FACE_OUTER_BOUND('',#820,.T.);
#439=FACE_OUTER_BOUND('',#821,.T.);
#440=FACE_OUTER_BOUND('',#822,.T.);
#441=FACE_OUTER_BOUND('',#823,.T.);
#442=FACE_OUTER_BOUND('',#824,.T.);
#443=FACE_OUTER_BOUND('',#826,.T.);
#444=FACE_OUTER_BOUND('',#828,.T.);
#445=FACE_OUTER_BOUND('',#829,.T.);
#446=FACE_OUTER_BOUND('',#830,.T.);
#447=FACE_OUTER_BOUND('',#831,.T.);
#448=FACE_OUTER_BOUND('',#832,.T.);
#449=FACE_OUTER_BOUND('',#833,.T.);
#450=FACE_OUTER_BOUND('',#834,.T.);
#451=FACE_OUTER_BOUND('',#835,.T.);
#452=FACE_OUTER_BOUND('',#836,.T.);
#453=FACE_OUTER_BOUND('',#837,.T.);
#454=FACE_OUTER_BOUND('',#838,.T.);
#455=FACE_OUTER_BOUND('',#839,.T.);
#456=FACE_OUTER_BOUND('',#840,.T.);
#457=FACE_OUTER_BOUND('',#841,.T.);
#458=FACE_OUTER_BOUND('',#842,.T.);
#459=FACE_OUTER_BOUND('',#843,.T.);
#460=FACE_OUTER_BOUND('',#844,.T.);
#461=FACE_OUTER_BOUND('',#845,.T.);
#462=FACE_OUTER_BOUND('',#846,.T.);
#463=FACE_OUTER_BOUND('',#847,.T.);
#464=FACE_OUTER_BOUND('',#848,.T.);
#465=FACE_OUTER_BOUND('',#849,.T.);
#466=FACE_OUTER_BOUND('',#850,.T.);
#467=FACE_OUTER_BOUND('',#851,.T.);
#468=FACE_OUTER_BOUND('',#852,.T.);
#469=FACE_OUTER_BOUND('',#853,.T.);
#470=FACE_OUTER_BOUND('',#854,.T.);
#471=FACE_OUTER_BOUND('',#855,.T.);
#472=FACE_OUTER_BOUND('',#856,.T.);
#473=FACE_OUTER_BOUND('',#857,.T.);
#474=FACE_OUTER_BOUND('',#858,.T.);
#475=FACE_OUTER_BOUND('',#859,.T.);
#476=FACE_OUTER_BOUND('',#860,.T.);
#477=FACE_OUTER_BOUND('',#861,.T.);
#478=FACE_OUTER_BOUND('',#862,.T.);
#479=FACE_OUTER_BOUND('',#863,.T.);
#480=FACE_OUTER_BOUND('',#864,.T.);
#481=FACE_OUTER_BOUND('',#865,.T.);
#482=FACE_OUTER_BOUND('',#866,.T.);
#483=FACE_OUTER_BOUND('',#867,.T.);
#484=FACE_OUTER_BOUND('',#868,.T.);
#485=FACE_OUTER_BOUND('',#869,.T.);
#486=FACE_OUTER_BOUND('',#870,.T.);
#487=FACE_OUTER_BOUND('',#871,.T.);
#488=FACE_OUTER_BOUND('',#872,.T.);
#489=FACE_OUTER_BOUND('',#873,.T.);
#490=FACE_OUTER_BOUND('',#874,.T.);
#491=FACE_OUTER_BOUND('',#875,.T.);
#492=FACE_OUTER_BOUND('',#876,.T.);
#493=FACE_OUTER_BOUND('',#877,.T.);
#494=FACE_OUTER_BOUND('',#878,.T.);
#495=FACE_OUTER_BOUND('',#879,.T.);
#496=FACE_OUTER_BOUND('',#880,.T.);
#497=FACE_OUTER_BOUND('',#881,.T.);
#498=FACE_OUTER_BOUND('',#882,.T.);
#499=FACE_OUTER_BOUND('',#883,.T.);
#500=FACE_OUTER_BOUND('',#884,.T.);
#501=FACE_OUTER_BOUND('',#885,.T.);
#502=FACE_OUTER_BOUND('',#886,.T.);
#503=FACE_OUTER_BOUND('',#887,.T.);
#504=FACE_OUTER_BOUND('',#888,.T.);
#505=FACE_OUTER_BOUND('',#889,.T.);
#506=FACE_OUTER_BOUND('',#890,.T.);
#507=FACE_OUTER_BOUND('',#891,.T.);
#508=FACE_OUTER_BOUND('',#892,.T.);
#509=FACE_OUTER_BOUND('',#893,.T.);
#510=FACE_OUTER_BOUND('',#894,.T.);
#511=FACE_OUTER_BOUND('',#895,.T.);
#512=FACE_OUTER_BOUND('',#896,.T.);
#513=FACE_OUTER_BOUND('',#897,.T.);
#514=FACE_OUTER_BOUND('',#898,.T.);
#515=FACE_OUTER_BOUND('',#899,.T.);
#516=FACE_OUTER_BOUND('',#900,.T.);
#517=FACE_OUTER_BOUND('',#901,.T.);
#518=FACE_OUTER_BOUND('',#902,.T.);
#519=FACE_OUTER_BOUND('',#903,.T.);
#520=FACE_OUTER_BOUND('',#904,.T.);
#521=FACE_OUTER_BOUND('',#905,.T.);
#522=FACE_OUTER_BOUND('',#906,.T.);
#523=FACE_OUTER_BOUND('',#907,.T.);
#524=FACE_OUTER_BOUND('',#908,.T.);
#525=FACE_OUTER_BOUND('',#909,.T.);
#526=FACE_OUTER_BOUND('',#910,.T.);
#527=FACE_OUTER_BOUND('',#911,.T.);
#528=FACE_OUTER_BOUND('',#912,.T.);
#529=FACE_OUTER_BOUND('',#913,.T.);
#530=FACE_OUTER_BOUND('',#914,.T.);
#531=FACE_OUTER_BOUND('',#915,.T.);
#532=FACE_OUTER_BOUND('',#916,.T.);
#533=FACE_OUTER_BOUND('',#917,.T.);
#534=FACE_OUTER_BOUND('',#918,.T.);
#535=FACE_OUTER_BOUND('',#919,.T.);
#536=FACE_OUTER_BOUND('',#920,.T.);
#537=FACE_OUTER_BOUND('',#921,.T.);
#538=FACE_OUTER_BOUND('',#922,.T.);
#539=FACE_OUTER_BOUND('',#923,.T.);
#540=FACE_OUTER_BOUND('',#924,.T.);
#541=FACE_OUTER_BOUND('',#925,.T.);
#542=FACE_OUTER_BOUND('',#926,.T.);
#543=FACE_OUTER_BOUND('',#927,.T.);
#544=FACE_OUTER_BOUND('',#928,.T.);
#545=FACE_OUTER_BOUND('',#929,.T.);
#546=FACE_OUTER_BOUND('',#930,.T.);
#547=FACE_OUTER_BOUND('',#931,.T.);
#548=FACE_OUTER_BOUND('',#932,.T.);
#549=FACE_OUTER_BOUND('',#933,.T.);
#550=FACE_OUTER_BOUND('',#934,.T.);
#551=FACE_OUTER_BOUND('',#935,.T.);
#552=FACE_OUTER_BOUND('',#936,.T.);
#553=FACE_OUTER_BOUND('',#937,.T.);
#554=FACE_OUTER_BOUND('',#938,.T.);
#555=FACE_OUTER_BOUND('',#939,.T.);
#556=FACE_OUTER_BOUND('',#940,.T.);
#557=FACE_OUTER_BOUND('',#941,.T.);
#558=FACE_OUTER_BOUND('',#942,.T.);
#559=FACE_OUTER_BOUND('',#943,.T.);
#560=FACE_OUTER_BOUND('',#944,.T.);
#561=FACE_OUTER_BOUND('',#945,.T.);
#562=FACE_OUTER_BOUND('',#946,.T.);
#563=FACE_OUTER_BOUND('',#947,.T.);
#564=FACE_OUTER_BOUND('',#948,.T.);
#565=FACE_OUTER_BOUND('',#949,.T.);
#566=FACE_OUTER_BOUND('',#950,.T.);
#567=FACE_OUTER_BOUND('',#951,.T.);
#568=FACE_OUTER_BOUND('',#952,.T.);
#569=FACE_OUTER_BOUND('',#953,.T.);
#570=FACE_OUTER_BOUND('',#954,.T.);
#571=FACE_OUTER_BOUND('',#955,.T.);
#572=FACE_OUTER_BOUND('',#956,.T.);
#573=FACE_OUTER_BOUND('',#957,.T.);
#574=FACE_OUTER_BOUND('',#958,.T.);
#575=FACE_OUTER_BOUND('',#959,.T.);
#576=FACE_OUTER_BOUND('',#960,.T.);
#577=FACE_OUTER_BOUND('',#961,.T.);
#578=FACE_OUTER_BOUND('',#962,.T.);
#579=FACE_OUTER_BOUND('',#963,.T.);
#580=FACE_OUTER_BOUND('',#964,.T.);
#581=FACE_OUTER_BOUND('',#965,.T.);
#582=FACE_OUTER_BOUND('',#966,.T.);
#583=FACE_OUTER_BOUND('',#967,.T.);
#584=FACE_OUTER_BOUND('',#970,.T.);
#585=FACE_OUTER_BOUND('',#971,.T.);
#586=FACE_OUTER_BOUND('',#974,.T.);
#587=FACE_OUTER_BOUND('',#975,.T.);
#588=FACE_OUTER_BOUND('',#976,.T.);
#589=FACE_OUTER_BOUND('',#977,.T.);
#590=FACE_OUTER_BOUND('',#978,.T.);
#591=FACE_OUTER_BOUND('',#979,.T.);
#592=FACE_OUTER_BOUND('',#980,.T.);
#593=FACE_OUTER_BOUND('',#981,.T.);
#594=FACE_OUTER_BOUND('',#982,.T.);
#595=FACE_OUTER_BOUND('',#983,.T.);
#596=FACE_OUTER_BOUND('',#984,.T.);
#597=FACE_OUTER_BOUND('',#985,.T.);
#598=FACE_OUTER_BOUND('',#986,.T.);
#599=FACE_OUTER_BOUND('',#987,.T.);
#600=FACE_OUTER_BOUND('',#988,.T.);
#601=FACE_OUTER_BOUND('',#989,.T.);
#602=FACE_OUTER_BOUND('',#990,.T.);
#603=FACE_OUTER_BOUND('',#991,.T.);
#604=FACE_OUTER_BOUND('',#992,.T.);
#605=FACE_OUTER_BOUND('',#993,.T.);
#606=FACE_OUTER_BOUND('',#994,.T.);
#607=FACE_OUTER_BOUND('',#995,.T.);
#608=FACE_OUTER_BOUND('',#996,.T.);
#609=FACE_OUTER_BOUND('',#997,.T.);
#610=FACE_OUTER_BOUND('',#999,.T.);
#611=FACE_OUTER_BOUND('',#1001,.T.);
#612=FACE_OUTER_BOUND('',#1002,.T.);
#613=FACE_OUTER_BOUND('',#1003,.T.);
#614=FACE_OUTER_BOUND('',#1004,.T.);
#615=FACE_OUTER_BOUND('',#1005,.T.);
#616=FACE_OUTER_BOUND('',#1006,.T.);
#617=FACE_OUTER_BOUND('',#1007,.T.);
#618=FACE_OUTER_BOUND('',#1008,.T.);
#619=FACE_OUTER_BOUND('',#1009,.T.);
#620=FACE_OUTER_BOUND('',#1010,.T.);
#621=FACE_OUTER_BOUND('',#1011,.T.);
#622=FACE_OUTER_BOUND('',#1012,.T.);
#623=FACE_OUTER_BOUND('',#1013,.T.);
#624=FACE_OUTER_BOUND('',#1014,.T.);
#625=FACE_OUTER_BOUND('',#1015,.T.);
#626=FACE_OUTER_BOUND('',#1016,.T.);
#627=FACE_OUTER_BOUND('',#1017,.T.);
#628=FACE_OUTER_BOUND('',#1018,.T.);
#629=FACE_OUTER_BOUND('',#1022,.T.);
#630=FACE_OUTER_BOUND('',#1023,.T.);
#631=FACE_OUTER_BOUND('',#1024,.T.);
#632=FACE_OUTER_BOUND('',#1025,.T.);
#633=FACE_OUTER_BOUND('',#1029,.T.);
#634=FACE_OUTER_BOUND('',#1030,.T.);
#635=FACE_OUTER_BOUND('',#1031,.T.);
#636=FACE_OUTER_BOUND('',#1032,.T.);
#637=FACE_OUTER_BOUND('',#1033,.T.);
#638=FACE_OUTER_BOUND('',#1034,.T.);
#639=FACE_OUTER_BOUND('',#1035,.T.);
#640=FACE_OUTER_BOUND('',#1036,.T.);
#641=FACE_OUTER_BOUND('',#1037,.T.);
#642=FACE_OUTER_BOUND('',#1038,.T.);
#643=FACE_OUTER_BOUND('',#1039,.T.);
#644=FACE_OUTER_BOUND('',#1040,.T.);
#645=FACE_OUTER_BOUND('',#1041,.T.);
#646=FACE_OUTER_BOUND('',#1043,.T.);
#647=FACE_OUTER_BOUND('',#1044,.T.);
#648=FACE_OUTER_BOUND('',#1045,.T.);
#649=FACE_OUTER_BOUND('',#1046,.T.);
#650=FACE_OUTER_BOUND('',#1047,.T.);
#651=FACE_OUTER_BOUND('',#1048,.T.);
#652=FACE_OUTER_BOUND('',#1049,.T.);
#653=FACE_OUTER_BOUND('',#1050,.T.);
#654=FACE_OUTER_BOUND('',#1052,.T.);
#655=FACE_OUTER_BOUND('',#1053,.T.);
#656=FACE_OUTER_BOUND('',#1054,.T.);
#657=FACE_OUTER_BOUND('',#1055,.T.);
#658=FACE_OUTER_BOUND('',#1056,.T.);
#659=FACE_OUTER_BOUND('',#1057,.T.);
#660=FACE_OUTER_BOUND('',#1058,.T.);
#661=FACE_OUTER_BOUND('',#1059,.T.);
#662=FACE_OUTER_BOUND('',#1060,.T.);
#663=FACE_OUTER_BOUND('',#1061,.T.);
#664=FACE_OUTER_BOUND('',#1062,.T.);
#665=FACE_OUTER_BOUND('',#1063,.T.);
#666=FACE_OUTER_BOUND('',#1065,.T.);
#667=FACE_OUTER_BOUND('',#1066,.T.);
#668=FACE_OUTER_BOUND('',#1067,.T.);
#669=FACE_OUTER_BOUND('',#1068,.T.);
#670=FACE_OUTER_BOUND('',#1069,.T.);
#671=FACE_OUTER_BOUND('',#1070,.T.);
#672=FACE_OUTER_BOUND('',#1071,.T.);
#673=EDGE_LOOP('',(#4112,#4113,#4114,#4115));
#674=EDGE_LOOP('',(#4116,#4117,#4118,#4119));
#675=EDGE_LOOP('',(#4120,#4121,#4122,#4123));
#676=EDGE_LOOP('',(#4124,#4125,#4126,#4127));
#677=EDGE_LOOP('',(#4128,#4129,#4130,#4131));
#678=EDGE_LOOP('',(#4132,#4133,#4134,#4135));
#679=EDGE_LOOP('',(#4136,#4137,#4138,#4139));
#680=EDGE_LOOP('',(#4140,#4141,#4142,#4143));
#681=EDGE_LOOP('',(#4144,#4145,#4146,#4147));
#682=EDGE_LOOP('',(#4148,#4149,#4150,#4151));
#683=EDGE_LOOP('',(#4152,#4153,#4154,#4155));
#684=EDGE_LOOP('',(#4156,#4157,#4158,#4159));
#685=EDGE_LOOP('',(#4160,#4161,#4162,#4163));
#686=EDGE_LOOP('',(#4164,#4165,#4166,#4167));
#687=EDGE_LOOP('',(#4168,#4169,#4170,#4171));
#688=EDGE_LOOP('',(#4172,#4173,#4174,#4175));
#689=EDGE_LOOP('',(#4176,#4177,#4178,#4179));
#690=EDGE_LOOP('',(#4180,#4181,#4182,#4183));
#691=EDGE_LOOP('',(#4184,#4185,#4186,#4187,#4188,#4189,#4190,#4191));
#692=EDGE_LOOP('',(#4192));
#693=EDGE_LOOP('',(#4193));
#694=EDGE_LOOP('',(#4194));
#695=EDGE_LOOP('',(#4195));
#696=EDGE_LOOP('',(#4196,#4197,#4198,#4199));
#697=EDGE_LOOP('',(#4200,#4201,#4202,#4203));
#698=EDGE_LOOP('',(#4204,#4205,#4206,#4207,#4208,#4209,#4210,#4211));
#699=EDGE_LOOP('',(#4212));
#700=EDGE_LOOP('',(#4213));
#701=EDGE_LOOP('',(#4214));
#702=EDGE_LOOP('',(#4215));
#703=EDGE_LOOP('',(#4216,#4217,#4218,#4219));
#704=EDGE_LOOP('',(#4220,#4221,#4222,#4223));
#705=EDGE_LOOP('',(#4224,#4225,#4226,#4227));
#706=EDGE_LOOP('',(#4228,#4229,#4230,#4231));
#707=EDGE_LOOP('',(#4232,#4233,#4234,#4235));
#708=EDGE_LOOP('',(#4236,#4237,#4238,#4239));
#709=EDGE_LOOP('',(#4240,#4241,#4242,#4243));
#710=EDGE_LOOP('',(#4244,#4245,#4246,#4247));
#711=EDGE_LOOP('',(#4248,#4249,#4250,#4251));
#712=EDGE_LOOP('',(#4252,#4253,#4254,#4255,#4256,#4257));
#713=EDGE_LOOP('',(#4258,#4259,#4260,#4261,#4262,#4263,#4264,#4265));
#714=EDGE_LOOP('',(#4266,#4267,#4268,#4269));
#715=EDGE_LOOP('',(#4270));
#716=EDGE_LOOP('',(#4271,#4272,#4273,#4274));
#717=EDGE_LOOP('',(#4275));
#718=EDGE_LOOP('',(#4276,#4277,#4278,#4279));
#719=EDGE_LOOP('',(#4280));
#720=EDGE_LOOP('',(#4281,#4282,#4283,#4284));
#721=EDGE_LOOP('',(#4285,#4286,#4287,#4288));
#722=EDGE_LOOP('',(#4289,#4290,#4291,#4292));
#723=EDGE_LOOP('',(#4293,#4294,#4295,#4296));
#724=EDGE_LOOP('',(#4297,#4298,#4299,#4300));
#725=EDGE_LOOP('',(#4301,#4302,#4303,#4304));
#726=EDGE_LOOP('',(#4305,#4306,#4307,#4308));
#727=EDGE_LOOP('',(#4309,#4310,#4311,#4312));
#728=EDGE_LOOP('',(#4313,#4314,#4315,#4316));
#729=EDGE_LOOP('',(#4317,#4318,#4319,#4320));
#730=EDGE_LOOP('',(#4321,#4322,#4323,#4324));
#731=EDGE_LOOP('',(#4325,#4326,#4327,#4328));
#732=EDGE_LOOP('',(#4329,#4330,#4331,#4332,#4333));
#733=EDGE_LOOP('',(#4334,#4335,#4336,#4337));
#734=EDGE_LOOP('',(#4338,#4339,#4340,#4341,#4342));
#735=EDGE_LOOP('',(#4343,#4344,#4345,#4346));
#736=EDGE_LOOP('',(#4347,#4348,#4349,#4350));
#737=EDGE_LOOP('',(#4351));
#738=EDGE_LOOP('',(#4352));
#739=EDGE_LOOP('',(#4353));
#740=EDGE_LOOP('',(#4354,#4355,#4356,#4357));
#741=EDGE_LOOP('',(#4358,#4359,#4360,#4361));
#742=EDGE_LOOP('',(#4362,#4363,#4364,#4365));
#743=EDGE_LOOP('',(#4366,#4367,#4368,#4369));
#744=EDGE_LOOP('',(#4370,#4371,#4372,#4373));
#745=EDGE_LOOP('',(#4374,#4375,#4376,#4377));
#746=EDGE_LOOP('',(#4378,#4379,#4380,#4381));
#747=EDGE_LOOP('',(#4382,#4383,#4384,#4385));
#748=EDGE_LOOP('',(#4386));
#749=EDGE_LOOP('',(#4387,#4388,#4389,#4390,#4391,#4392,#4393,#4394));
#750=EDGE_LOOP('',(#4395,#4396,#4397,#4398));
#751=EDGE_LOOP('',(#4399));
#752=EDGE_LOOP('',(#4400,#4401,#4402,#4403));
#753=EDGE_LOOP('',(#4404));
#754=EDGE_LOOP('',(#4405,#4406,#4407,#4408));
#755=EDGE_LOOP('',(#4409));
#756=EDGE_LOOP('',(#4410));
#757=EDGE_LOOP('',(#4411,#4412,#4413,#4414,#4415,#4416));
#758=EDGE_LOOP('',(#4417,#4418,#4419,#4420));
#759=EDGE_LOOP('',(#4421,#4422,#4423,#4424,#4425,#4426));
#760=EDGE_LOOP('',(#4427,#4428,#4429,#4430));
#761=EDGE_LOOP('',(#4431,#4432,#4433,#4434));
#762=EDGE_LOOP('',(#4435,#4436,#4437,#4438));
#763=EDGE_LOOP('',(#4439,#4440,#4441,#4442));
#764=EDGE_LOOP('',(#4443,#4444,#4445,#4446));
#765=EDGE_LOOP('',(#4447,#4448,#4449,#4450));
#766=EDGE_LOOP('',(#4451,#4452,#4453,#4454));
#767=EDGE_LOOP('',(#4455,#4456,#4457,#4458));
#768=EDGE_LOOP('',(#4459,#4460,#4461,#4462));
#769=EDGE_LOOP('',(#4463,#4464,#4465,#4466));
#770=EDGE_LOOP('',(#4467,#4468,#4469,#4470));
#771=EDGE_LOOP('',(#4471,#4472,#4473,#4474,#4475,#4476,#4477,#4478));
#772=EDGE_LOOP('',(#4479,#4480,#4481,#4482));
#773=EDGE_LOOP('',(#4483));
#774=EDGE_LOOP('',(#4484));
#775=EDGE_LOOP('',(#4485));
#776=EDGE_LOOP('',(#4486,#4487,#4488,#4489));
#777=EDGE_LOOP('',(#4490,#4491,#4492,#4493));
#778=EDGE_LOOP('',(#4494,#4495,#4496,#4497));
#779=EDGE_LOOP('',(#4498,#4499,#4500,#4501));
#780=EDGE_LOOP('',(#4502,#4503,#4504,#4505));
#781=EDGE_LOOP('',(#4506,#4507,#4508,#4509));
#782=EDGE_LOOP('',(#4510,#4511,#4512,#4513));
#783=EDGE_LOOP('',(#4514,#4515,#4516,#4517));
#784=EDGE_LOOP('',(#4518,#4519,#4520,#4521));
#785=EDGE_LOOP('',(#4522,#4523,#4524,#4525));
#786=EDGE_LOOP('',(#4526,#4527,#4528,#4529));
#787=EDGE_LOOP('',(#4530,#4531,#4532,#4533));
#788=EDGE_LOOP('',(#4534,#4535,#4536,#4537));
#789=EDGE_LOOP('',(#4538,#4539,#4540,#4541));
#790=EDGE_LOOP('',(#4542,#4543,#4544,#4545));
#791=EDGE_LOOP('',(#4546,#4547,#4548,#4549));
#792=EDGE_LOOP('',(#4550,#4551,#4552,#4553));
#793=EDGE_LOOP('',(#4554,#4555,#4556,#4557));
#794=EDGE_LOOP('',(#4558,#4559,#4560,#4561));
#795=EDGE_LOOP('',(#4562,#4563,#4564,#4565));
#796=EDGE_LOOP('',(#4566,#4567,#4568,#4569));
#797=EDGE_LOOP('',(#4570,#4571,#4572,#4573));
#798=EDGE_LOOP('',(#4574,#4575,#4576,#4577));
#799=EDGE_LOOP('',(#4578,#4579,#4580,#4581));
#800=EDGE_LOOP('',(#4582,#4583,#4584,#4585));
#801=EDGE_LOOP('',(#4586,#4587,#4588,#4589));
#802=EDGE_LOOP('',(#4590,#4591,#4592,#4593));
#803=EDGE_LOOP('',(#4594,#4595,#4596,#4597));
#804=EDGE_LOOP('',(#4598,#4599,#4600,#4601));
#805=EDGE_LOOP('',(#4602,#4603,#4604,#4605));
#806=EDGE_LOOP('',(#4606,#4607,#4608,#4609));
#807=EDGE_LOOP('',(#4610,#4611,#4612,#4613));
#808=EDGE_LOOP('',(#4614,#4615,#4616,#4617));
#809=EDGE_LOOP('',(#4618,#4619,#4620,#4621));
#810=EDGE_LOOP('',(#4622,#4623,#4624,#4625));
#811=EDGE_LOOP('',(#4626,#4627,#4628,#4629));
#812=EDGE_LOOP('',(#4630,#4631,#4632,#4633));
#813=EDGE_LOOP('',(#4634,#4635,#4636,#4637));
#814=EDGE_LOOP('',(#4638,#4639,#4640,#4641));
#815=EDGE_LOOP('',(#4642,#4643,#4644,#4645));
#816=EDGE_LOOP('',(#4646,#4647,#4648,#4649));
#817=EDGE_LOOP('',(#4650,#4651,#4652,#4653));
#818=EDGE_LOOP('',(#4654,#4655,#4656,#4657));
#819=EDGE_LOOP('',(#4658,#4659,#4660,#4661));
#820=EDGE_LOOP('',(#4662,#4663,#4664,#4665));
#821=EDGE_LOOP('',(#4666,#4667,#4668,#4669));
#822=EDGE_LOOP('',(#4670,#4671,#4672,#4673));
#823=EDGE_LOOP('',(#4674,#4675,#4676,#4677));
#824=EDGE_LOOP('',(#4678,#4679,#4680,#4681,#4682,#4683,#4684,#4685,#4686,
#4687,#4688,#4689,#4690,#4691,#4692,#4693,#4694,#4695,#4696,#4697,#4698,
#4699,#4700,#4701,#4702,#4703,#4704,#4705,#4706,#4707,#4708,#4709,#4710,
#4711,#4712,#4713,#4714,#4715,#4716,#4717,#4718,#4719,#4720,#4721,#4722,
#4723,#4724,#4725,#4726,#4727,#4728,#4729,#4730,#4731,#4732,#4733,#4734,
#4735,#4736,#4737,#4738,#4739,#4740,#4741,#4742,#4743,#4744,#4745,#4746,
#4747,#4748,#4749,#4750,#4751,#4752,#4753,#4754,#4755,#4756,#4757,#4758,
#4759,#4760,#4761,#4762,#4763,#4764,#4765,#4766,#4767,#4768,#4769,#4770,
#4771,#4772,#4773,#4774,#4775,#4776,#4777,#4778,#4779,#4780,#4781,#4782,
#4783,#4784,#4785,#4786,#4787,#4788,#4789,#4790,#4791,#4792,#4793,#4794,
#4795,#4796,#4797,#4798,#4799,#4800,#4801,#4802,#4803,#4804,#4805,#4806,
#4807,#4808,#4809,#4810,#4811,#4812,#4813,#4814,#4815,#4816,#4817,#4818,
#4819,#4820,#4821,#4822,#4823,#4824,#4825,#4826,#4827,#4828,#4829,#4830,
#4831,#4832,#4833,#4834,#4835,#4836,#4837,#4838,#4839,#4840,#4841,#4842,
#4843,#4844,#4845,#4846,#4847,#4848,#4849,#4850,#4851,#4852,#4853,#4854,
#4855,#4856,#4857));
#825=EDGE_LOOP('',(#4858,#4859,#4860,#4861));
#826=EDGE_LOOP('',(#4862,#4863,#4864,#4865,#4866,#4867,#4868,#4869,#4870,
#4871,#4872,#4873,#4874,#4875,#4876,#4877,#4878,#4879,#4880,#4881,#4882,
#4883,#4884,#4885,#4886,#4887,#4888,#4889,#4890,#4891,#4892,#4893,#4894,
#4895,#4896,#4897,#4898,#4899,#4900,#4901,#4902,#4903,#4904,#4905,#4906,
#4907,#4908,#4909,#4910,#4911,#4912,#4913,#4914,#4915,#4916,#4917,#4918,
#4919,#4920,#4921,#4922,#4923,#4924,#4925,#4926,#4927,#4928,#4929,#4930,
#4931,#4932,#4933,#4934,#4935,#4936,#4937,#4938,#4939,#4940,#4941,#4942,
#4943,#4944,#4945,#4946,#4947,#4948,#4949,#4950,#4951,#4952,#4953,#4954,
#4955,#4956,#4957,#4958,#4959,#4960,#4961,#4962,#4963,#4964,#4965,#4966,
#4967,#4968,#4969,#4970,#4971,#4972,#4973,#4974,#4975,#4976,#4977,#4978,
#4979,#4980,#4981,#4982,#4983,#4984,#4985,#4986,#4987,#4988,#4989,#4990,
#4991,#4992,#4993,#4994,#4995,#4996,#4997,#4998,#4999,#5000,#5001,#5002,
#5003,#5004,#5005,#5006,#5007,#5008,#5009,#5010,#5011,#5012,#5013,#5014,
#5015,#5016,#5017,#5018,#5019,#5020,#5021,#5022,#5023,#5024,#5025,#5026,
#5027,#5028,#5029,#5030,#5031,#5032,#5033,#5034,#5035,#5036,#5037,#5038,
#5039,#5040,#5041));
#827=EDGE_LOOP('',(#5042,#5043,#5044,#5045));
#828=EDGE_LOOP('',(#5046,#5047,#5048,#5049));
#829=EDGE_LOOP('',(#5050,#5051,#5052,#5053));
#830=EDGE_LOOP('',(#5054,#5055,#5056,#5057));
#831=EDGE_LOOP('',(#5058,#5059,#5060,#5061));
#832=EDGE_LOOP('',(#5062,#5063,#5064,#5065));
#833=EDGE_LOOP('',(#5066,#5067,#5068,#5069));
#834=EDGE_LOOP('',(#5070,#5071,#5072,#5073));
#835=EDGE_LOOP('',(#5074,#5075,#5076,#5077));
#836=EDGE_LOOP('',(#5078,#5079,#5080,#5081));
#837=EDGE_LOOP('',(#5082,#5083,#5084,#5085));
#838=EDGE_LOOP('',(#5086,#5087,#5088,#5089));
#839=EDGE_LOOP('',(#5090,#5091,#5092,#5093));
#840=EDGE_LOOP('',(#5094,#5095,#5096,#5097));
#841=EDGE_LOOP('',(#5098,#5099,#5100,#5101));
#842=EDGE_LOOP('',(#5102,#5103,#5104,#5105));
#843=EDGE_LOOP('',(#5106,#5107,#5108,#5109));
#844=EDGE_LOOP('',(#5110,#5111,#5112,#5113));
#845=EDGE_LOOP('',(#5114,#5115,#5116,#5117));
#846=EDGE_LOOP('',(#5118,#5119,#5120,#5121));
#847=EDGE_LOOP('',(#5122,#5123,#5124,#5125));
#848=EDGE_LOOP('',(#5126,#5127,#5128,#5129));
#849=EDGE_LOOP('',(#5130,#5131,#5132,#5133));
#850=EDGE_LOOP('',(#5134,#5135,#5136,#5137));
#851=EDGE_LOOP('',(#5138,#5139,#5140,#5141));
#852=EDGE_LOOP('',(#5142,#5143,#5144,#5145));
#853=EDGE_LOOP('',(#5146,#5147,#5148,#5149));
#854=EDGE_LOOP('',(#5150,#5151,#5152,#5153));
#855=EDGE_LOOP('',(#5154,#5155,#5156,#5157));
#856=EDGE_LOOP('',(#5158,#5159,#5160,#5161));
#857=EDGE_LOOP('',(#5162,#5163,#5164,#5165));
#858=EDGE_LOOP('',(#5166,#5167,#5168,#5169));
#859=EDGE_LOOP('',(#5170,#5171,#5172,#5173));
#860=EDGE_LOOP('',(#5174,#5175,#5176,#5177));
#861=EDGE_LOOP('',(#5178,#5179,#5180,#5181));
#862=EDGE_LOOP('',(#5182,#5183,#5184,#5185));
#863=EDGE_LOOP('',(#5186,#5187,#5188,#5189));
#864=EDGE_LOOP('',(#5190,#5191,#5192,#5193));
#865=EDGE_LOOP('',(#5194,#5195,#5196,#5197));
#866=EDGE_LOOP('',(#5198,#5199,#5200,#5201));
#867=EDGE_LOOP('',(#5202,#5203,#5204,#5205));
#868=EDGE_LOOP('',(#5206,#5207,#5208,#5209));
#869=EDGE_LOOP('',(#5210,#5211,#5212,#5213));
#870=EDGE_LOOP('',(#5214,#5215,#5216,#5217));
#871=EDGE_LOOP('',(#5218,#5219,#5220,#5221));
#872=EDGE_LOOP('',(#5222,#5223,#5224,#5225));
#873=EDGE_LOOP('',(#5226,#5227,#5228,#5229));
#874=EDGE_LOOP('',(#5230,#5231,#5232,#5233));
#875=EDGE_LOOP('',(#5234,#5235,#5236,#5237));
#876=EDGE_LOOP('',(#5238,#5239,#5240,#5241));
#877=EDGE_LOOP('',(#5242,#5243,#5244,#5245));
#878=EDGE_LOOP('',(#5246,#5247,#5248,#5249));
#879=EDGE_LOOP('',(#5250,#5251,#5252,#5253));
#880=EDGE_LOOP('',(#5254,#5255,#5256,#5257));
#881=EDGE_LOOP('',(#5258,#5259,#5260,#5261));
#882=EDGE_LOOP('',(#5262,#5263,#5264,#5265));
#883=EDGE_LOOP('',(#5266,#5267,#5268,#5269));
#884=EDGE_LOOP('',(#5270,#5271,#5272,#5273));
#885=EDGE_LOOP('',(#5274,#5275,#5276,#5277));
#886=EDGE_LOOP('',(#5278,#5279,#5280,#5281));
#887=EDGE_LOOP('',(#5282,#5283,#5284,#5285));
#888=EDGE_LOOP('',(#5286,#5287,#5288,#5289));
#889=EDGE_LOOP('',(#5290,#5291,#5292,#5293));
#890=EDGE_LOOP('',(#5294,#5295,#5296,#5297));
#891=EDGE_LOOP('',(#5298,#5299,#5300,#5301));
#892=EDGE_LOOP('',(#5302,#5303,#5304,#5305));
#893=EDGE_LOOP('',(#5306,#5307,#5308,#5309));
#894=EDGE_LOOP('',(#5310,#5311,#5312,#5313));
#895=EDGE_LOOP('',(#5314,#5315,#5316,#5317));
#896=EDGE_LOOP('',(#5318,#5319,#5320,#5321));
#897=EDGE_LOOP('',(#5322,#5323,#5324,#5325));
#898=EDGE_LOOP('',(#5326,#5327,#5328,#5329));
#899=EDGE_LOOP('',(#5330,#5331,#5332,#5333));
#900=EDGE_LOOP('',(#5334,#5335,#5336,#5337));
#901=EDGE_LOOP('',(#5338,#5339,#5340,#5341));
#902=EDGE_LOOP('',(#5342,#5343,#5344,#5345));
#903=EDGE_LOOP('',(#5346,#5347,#5348,#5349));
#904=EDGE_LOOP('',(#5350,#5351,#5352,#5353));
#905=EDGE_LOOP('',(#5354,#5355,#5356,#5357));
#906=EDGE_LOOP('',(#5358,#5359,#5360,#5361));
#907=EDGE_LOOP('',(#5362,#5363,#5364,#5365));
#908=EDGE_LOOP('',(#5366,#5367,#5368,#5369));
#909=EDGE_LOOP('',(#5370,#5371,#5372,#5373));
#910=EDGE_LOOP('',(#5374,#5375,#5376,#5377));
#911=EDGE_LOOP('',(#5378,#5379,#5380,#5381));
#912=EDGE_LOOP('',(#5382,#5383,#5384,#5385));
#913=EDGE_LOOP('',(#5386,#5387,#5388,#5389));
#914=EDGE_LOOP('',(#5390,#5391,#5392,#5393));
#915=EDGE_LOOP('',(#5394,#5395,#5396,#5397));
#916=EDGE_LOOP('',(#5398,#5399,#5400,#5401));
#917=EDGE_LOOP('',(#5402,#5403,#5404,#5405));
#918=EDGE_LOOP('',(#5406,#5407,#5408,#5409));
#919=EDGE_LOOP('',(#5410,#5411,#5412,#5413));
#920=EDGE_LOOP('',(#5414,#5415,#5416,#5417));
#921=EDGE_LOOP('',(#5418,#5419,#5420,#5421));
#922=EDGE_LOOP('',(#5422,#5423,#5424,#5425));
#923=EDGE_LOOP('',(#5426,#5427,#5428,#5429));
#924=EDGE_LOOP('',(#5430,#5431,#5432,#5433));
#925=EDGE_LOOP('',(#5434,#5435,#5436,#5437));
#926=EDGE_LOOP('',(#5438,#5439,#5440,#5441));
#927=EDGE_LOOP('',(#5442,#5443,#5444,#5445));
#928=EDGE_LOOP('',(#5446,#5447,#5448,#5449));
#929=EDGE_LOOP('',(#5450,#5451,#5452,#5453));
#930=EDGE_LOOP('',(#5454,#5455,#5456,#5457));
#931=EDGE_LOOP('',(#5458,#5459,#5460,#5461));
#932=EDGE_LOOP('',(#5462,#5463,#5464,#5465));
#933=EDGE_LOOP('',(#5466,#5467,#5468,#5469));
#934=EDGE_LOOP('',(#5470,#5471,#5472,#5473));
#935=EDGE_LOOP('',(#5474,#5475,#5476,#5477));
#936=EDGE_LOOP('',(#5478,#5479,#5480,#5481));
#937=EDGE_LOOP('',(#5482,#5483,#5484,#5485));
#938=EDGE_LOOP('',(#5486,#5487,#5488,#5489));
#939=EDGE_LOOP('',(#5490,#5491,#5492,#5493));
#940=EDGE_LOOP('',(#5494,#5495,#5496,#5497));
#941=EDGE_LOOP('',(#5498,#5499,#5500,#5501));
#942=EDGE_LOOP('',(#5502,#5503,#5504,#5505));
#943=EDGE_LOOP('',(#5506,#5507,#5508,#5509));
#944=EDGE_LOOP('',(#5510,#5511,#5512,#5513));
#945=EDGE_LOOP('',(#5514,#5515,#5516,#5517));
#946=EDGE_LOOP('',(#5518,#5519,#5520,#5521));
#947=EDGE_LOOP('',(#5522,#5523,#5524,#5525));
#948=EDGE_LOOP('',(#5526,#5527,#5528,#5529));
#949=EDGE_LOOP('',(#5530,#5531,#5532,#5533));
#950=EDGE_LOOP('',(#5534,#5535,#5536,#5537));
#951=EDGE_LOOP('',(#5538,#5539,#5540,#5541));
#952=EDGE_LOOP('',(#5542,#5543,#5544,#5545));
#953=EDGE_LOOP('',(#5546,#5547,#5548,#5549));
#954=EDGE_LOOP('',(#5550,#5551,#5552,#5553));
#955=EDGE_LOOP('',(#5554,#5555,#5556,#5557));
#956=EDGE_LOOP('',(#5558,#5559,#5560,#5561));
#957=EDGE_LOOP('',(#5562,#5563,#5564,#5565));
#958=EDGE_LOOP('',(#5566,#5567,#5568,#5569));
#959=EDGE_LOOP('',(#5570,#5571,#5572,#5573));
#960=EDGE_LOOP('',(#5574,#5575,#5576,#5577));
#961=EDGE_LOOP('',(#5578,#5579,#5580,#5581));
#962=EDGE_LOOP('',(#5582,#5583,#5584,#5585));
#963=EDGE_LOOP('',(#5586,#5587,#5588,#5589));
#964=EDGE_LOOP('',(#5590,#5591,#5592,#5593));
#965=EDGE_LOOP('',(#5594,#5595,#5596,#5597,#5598,#5599,#5600,#5601));
#966=EDGE_LOOP('',(#5602,#5603,#5604,#5605));
#967=EDGE_LOOP('',(#5606,#5607,#5608,#5609,#5610,#5611,#5612,#5613,#5614,
#5615,#5616));
#968=EDGE_LOOP('',(#5617));
#969=EDGE_LOOP('',(#5618));
#970=EDGE_LOOP('',(#5619,#5620,#5621,#5622,#5623,#5624));
#971=EDGE_LOOP('',(#5625,#5626,#5627,#5628,#5629,#5630,#5631,#5632,#5633,
#5634,#5635));
#972=EDGE_LOOP('',(#5636));
#973=EDGE_LOOP('',(#5637));
#974=EDGE_LOOP('',(#5638,#5639,#5640,#5641,#5642,#5643));
#975=EDGE_LOOP('',(#5644,#5645,#5646,#5647));
#976=EDGE_LOOP('',(#5648,#5649,#5650,#5651));
#977=EDGE_LOOP('',(#5652,#5653,#5654,#5655));
#978=EDGE_LOOP('',(#5656,#5657,#5658,#5659));
#979=EDGE_LOOP('',(#5660,#5661,#5662,#5663));
#980=EDGE_LOOP('',(#5664,#5665,#5666,#5667));
#981=EDGE_LOOP('',(#5668,#5669,#5670,#5671));
#982=EDGE_LOOP('',(#5672,#5673,#5674,#5675,#5676,#5677,#5678,#5679));
#983=EDGE_LOOP('',(#5680,#5681,#5682,#5683));
#984=EDGE_LOOP('',(#5684,#5685,#5686,#5687,#5688,#5689,#5690,#5691,#5692,
#5693,#5694,#5695));
#985=EDGE_LOOP('',(#5696,#5697,#5698,#5699));
#986=EDGE_LOOP('',(#5700,#5701,#5702,#5703));
#987=EDGE_LOOP('',(#5704,#5705,#5706,#5707));
#988=EDGE_LOOP('',(#5708,#5709,#5710,#5711));
#989=EDGE_LOOP('',(#5712,#5713,#5714,#5715));
#990=EDGE_LOOP('',(#5716,#5717,#5718,#5719));
#991=EDGE_LOOP('',(#5720,#5721,#5722,#5723));
#992=EDGE_LOOP('',(#5724,#5725,#5726,#5727));
#993=EDGE_LOOP('',(#5728,#5729,#5730,#5731,#5732,#5733,#5734,#5735,#5736,
#5737,#5738,#5739));
#994=EDGE_LOOP('',(#5740,#5741,#5742,#5743));
#995=EDGE_LOOP('',(#5744,#5745,#5746,#5747));
#996=EDGE_LOOP('',(#5748,#5749,#5750,#5751));
#997=EDGE_LOOP('',(#5752));
#998=EDGE_LOOP('',(#5753));
#999=EDGE_LOOP('',(#5754,#5755,#5756,#5757));
#1000=EDGE_LOOP('',(#5758));
#1001=EDGE_LOOP('',(#5759,#5760,#5761,#5762));
#1002=EDGE_LOOP('',(#5763,#5764,#5765,#5766));
#1003=EDGE_LOOP('',(#5767,#5768,#5769,#5770));
#1004=EDGE_LOOP('',(#5771,#5772,#5773,#5774));
#1005=EDGE_LOOP('',(#5775,#5776,#5777,#5778));
#1006=EDGE_LOOP('',(#5779,#5780,#5781,#5782,#5783));
#1007=EDGE_LOOP('',(#5784,#5785,#5786,#5787));
#1008=EDGE_LOOP('',(#5788,#5789,#5790,#5791,#5792,#5793,#5794,#5795));
#1009=EDGE_LOOP('',(#5796,#5797,#5798,#5799));
#1010=EDGE_LOOP('',(#5800,#5801,#5802,#5803));
#1011=EDGE_LOOP('',(#5804,#5805,#5806,#5807));
#1012=EDGE_LOOP('',(#5808,#5809,#5810,#5811));
#1013=EDGE_LOOP('',(#5812,#5813,#5814,#5815));
#1014=EDGE_LOOP('',(#5816,#5817,#5818,#5819));
#1015=EDGE_LOOP('',(#5820,#5821,#5822,#5823));
#1016=EDGE_LOOP('',(#5824,#5825,#5826,#5827));
#1017=EDGE_LOOP('',(#5828,#5829,#5830,#5831));
#1018=EDGE_LOOP('',(#5832,#5833,#5834,#5835));
#1019=EDGE_LOOP('',(#5836));
#1020=EDGE_LOOP('',(#5837));
#1021=EDGE_LOOP('',(#5838,#5839,#5840,#5841));
#1022=EDGE_LOOP('',(#5842,#5843,#5844,#5845));
#1023=EDGE_LOOP('',(#5846,#5847,#5848,#5849));
#1024=EDGE_LOOP('',(#5850,#5851,#5852,#5853));
#1025=EDGE_LOOP('',(#5854,#5855,#5856,#5857));
#1026=EDGE_LOOP('',(#5858,#5859,#5860,#5861));
#1027=EDGE_LOOP('',(#5862));
#1028=EDGE_LOOP('',(#5863));
#1029=EDGE_LOOP('',(#5864,#5865,#5866,#5867));
#1030=EDGE_LOOP('',(#5868,#5869,#5870,#5871));
#1031=EDGE_LOOP('',(#5872,#5873,#5874,#5875));
#1032=EDGE_LOOP('',(#5876,#5877,#5878,#5879));
#1033=EDGE_LOOP('',(#5880,#5881,#5882,#5883));
#1034=EDGE_LOOP('',(#5884,#5885,#5886,#5887));
#1035=EDGE_LOOP('',(#5888,#5889,#5890,#5891));
#1036=EDGE_LOOP('',(#5892,#5893,#5894,#5895));
#1037=EDGE_LOOP('',(#5896,#5897,#5898,#5899,#5900,#5901,#5902,#5903,#5904,
#5905,#5906,#5907));
#1038=EDGE_LOOP('',(#5908,#5909,#5910,#5911));
#1039=EDGE_LOOP('',(#5912,#5913,#5914,#5915));
#1040=EDGE_LOOP('',(#5916,#5917,#5918,#5919));
#1041=EDGE_LOOP('',(#5920));
#1042=EDGE_LOOP('',(#5921));
#1043=EDGE_LOOP('',(#5922,#5923,#5924,#5925,#5926));
#1044=EDGE_LOOP('',(#5927,#5928,#5929,#5930));
#1045=EDGE_LOOP('',(#5931,#5932,#5933,#5934,#5935,#5936,#5937,#5938));
#1046=EDGE_LOOP('',(#5939,#5940,#5941,#5942));
#1047=EDGE_LOOP('',(#5943,#5944,#5945,#5946));
#1048=EDGE_LOOP('',(#5947,#5948,#5949,#5950));
#1049=EDGE_LOOP('',(#5951,#5952,#5953,#5954));
#1050=EDGE_LOOP('',(#5955,#5956,#5957,#5958));
#1051=EDGE_LOOP('',(#5959));
#1052=EDGE_LOOP('',(#5960,#5961,#5962,#5963));
#1053=EDGE_LOOP('',(#5964,#5965,#5966,#5967));
#1054=EDGE_LOOP('',(#5968,#5969,#5970,#5971));
#1055=EDGE_LOOP('',(#5972,#5973,#5974,#5975));
#1056=EDGE_LOOP('',(#5976,#5977,#5978,#5979));
#1057=EDGE_LOOP('',(#5980,#5981,#5982,#5983,#5984));
#1058=EDGE_LOOP('',(#5985,#5986,#5987,#5988));
#1059=EDGE_LOOP('',(#5989,#5990,#5991,#5992,#5993));
#1060=EDGE_LOOP('',(#5994,#5995,#5996,#5997,#5998,#5999,#6000,#6001,#6002,
#6003,#6004,#6005));
#1061=EDGE_LOOP('',(#6006,#6007,#6008,#6009));
#1062=EDGE_LOOP('',(#6010,#6011,#6012,#6013));
#1063=EDGE_LOOP('',(#6014));
#1064=EDGE_LOOP('',(#6015,#6016,#6017,#6018,#6019,#6020,#6021,#6022,#6023));
#1065=EDGE_LOOP('',(#6024,#6025,#6026,#6027));
#1066=EDGE_LOOP('',(#6028,#6029,#6030,#6031));
#1067=EDGE_LOOP('',(#6032,#6033,#6034,#6035));
#1068=EDGE_LOOP('',(#6036,#6037,#6038,#6039));
#1069=EDGE_LOOP('',(#6040,#6041,#6042,#6043));
#1070=EDGE_LOOP('',(#6044));
#1071=EDGE_LOOP('',(#6045));
#1072=LINE('',#9914,#1534);
#1073=LINE('',#9920,#1535);
#1074=LINE('',#9926,#1536);
#1075=LINE('',#9932,#1537);
#1076=LINE('',#9937,#1538);
#1077=LINE('',#9939,#1539);
#1078=LINE('',#9941,#1540);
#1079=LINE('',#9942,#1541);
#1080=LINE('',#9945,#1542);
#1081=LINE('',#9947,#1543);
#1082=LINE('',#9948,#1544);
#1083=LINE('',#9951,#1545);
#1084=LINE('',#9953,#1546);
#1085=LINE('',#9954,#1547);
#1086=LINE('',#9957,#1548);
#1087=LINE('',#9959,#1549);
#1088=LINE('',#9960,#1550);
#1089=LINE('',#9964,#1551);
#1090=LINE('',#9966,#1552);
#1091=LINE('',#9968,#1553);
#1092=LINE('',#9969,#1554);
#1093=LINE('',#9975,#1555);
#1094=LINE('',#9978,#1556);
#1095=LINE('',#9983,#1557);
#1096=LINE('',#9987,#1558);
#1097=LINE('',#9989,#1559);
#1098=LINE('',#9990,#1560);
#1099=LINE('',#9996,#1561);
#1100=LINE('',#9999,#1562);
#1101=LINE('',#10004,#1563);
#1102=LINE('',#10010,#1564);
#1103=LINE('',#10014,#1565);
#1104=LINE('',#10016,#1566);
#1105=LINE('',#10017,#1567);
#1106=LINE('',#10022,#1568);
#1107=LINE('',#10023,#1569);
#1108=LINE('',#10037,#1570);
#1109=LINE('',#10044,#1571);
#1110=LINE('',#10047,#1572);
#1111=LINE('',#10053,#1573);
#1112=LINE('',#10056,#1574);
#1113=LINE('',#10061,#1575);
#1114=LINE('',#10067,#1576);
#1115=LINE('',#10076,#1577);
#1116=LINE('',#10080,#1578);
#1117=LINE('',#10086,#1579);
#1118=LINE('',#10088,#1580);
#1119=LINE('',#10091,#1581);
#1120=LINE('',#10092,#1582);
#1121=LINE('',#10096,#1583);
#1122=LINE('',#10097,#1584);
#1123=LINE('',#10100,#1585);
#1124=LINE('',#10103,#1586);
#1125=LINE('',#10105,#1587);
#1126=LINE('',#10108,#1588);
#1127=LINE('',#10110,#1589);
#1128=LINE('',#10112,#1590);
#1129=LINE('',#10116,#1591);
#1130=LINE('',#10119,#1592);
#1131=LINE('',#10121,#1593);
#1132=LINE('',#10123,#1594);
#1133=LINE('',#10127,#1595);
#1134=LINE('',#10128,#1596);
#1135=LINE('',#10132,#1597);
#1136=LINE('',#10134,#1598);
#1137=LINE('',#10138,#1599);
#1138=LINE('',#10140,#1600);
#1139=LINE('',#10141,#1601);
#1140=LINE('',#10144,#1602);
#1141=LINE('',#10146,#1603);
#1142=LINE('',#10147,#1604);
#1143=LINE('',#10150,#1605);
#1144=LINE('',#10154,#1606);
#1145=LINE('',#10155,#1607);
#1146=LINE('',#10157,#1608);
#1147=LINE('',#10165,#1609);
#1148=LINE('',#10172,#1610);
#1149=LINE('',#10175,#1611);
#1150=LINE('',#10180,#1612);
#1151=LINE('',#10187,#1613);
#1152=LINE('',#10190,#1614);
#1153=LINE('',#10196,#1615);
#1154=LINE('',#10199,#1616);
#1155=LINE('',#10204,#1617);
#1156=LINE('',#10210,#1618);
#1157=LINE('',#10214,#1619);
#1158=LINE('',#10216,#1620);
#1159=LINE('',#10217,#1621);
#1160=LINE('',#10223,#1622);
#1161=LINE('',#10225,#1623);
#1162=LINE('',#10227,#1624);
#1163=LINE('',#10231,#1625);
#1164=LINE('',#10233,#1626);
#1165=LINE('',#10234,#1627);
#1166=LINE('',#10238,#1628);
#1167=LINE('',#10239,#1629);
#1168=LINE('',#10242,#1630);
#1169=LINE('',#10244,#1631);
#1170=LINE('',#10247,#1632);
#1171=LINE('',#10250,#1633);
#1172=LINE('',#10252,#1634);
#1173=LINE('',#10253,#1635);
#1174=LINE('',#10255,#1636);
#1175=LINE('',#10257,#1637);
#1176=LINE('',#10260,#1638);
#1177=LINE('',#10263,#1639);
#1178=LINE('',#10265,#1640);
#1179=LINE('',#10267,#1641);
#1180=LINE('',#10271,#1642);
#1181=LINE('',#10272,#1643);
#1182=LINE('',#10276,#1644);
#1183=LINE('',#10278,#1645);
#1184=LINE('',#10282,#1646);
#1185=LINE('',#10284,#1647);
#1186=LINE('',#10285,#1648);
#1187=LINE('',#10288,#1649);
#1188=LINE('',#10292,#1650);
#1189=LINE('',#10293,#1651);
#1190=LINE('',#10295,#1652);
#1191=LINE('',#10304,#1653);
#1192=LINE('',#10307,#1654);
#1193=LINE('',#10313,#1655);
#1194=LINE('',#10316,#1656);
#1195=LINE('',#10321,#1657);
#1196=LINE('',#10328,#1658);
#1197=LINE('',#10331,#1659);
#1198=LINE('',#10336,#1660);
#1199=LINE('',#10343,#1661);
#1200=LINE('',#10346,#1662);
#1201=LINE('',#10352,#1663);
#1202=LINE('',#10358,#1664);
#1203=LINE('',#10361,#1665);
#1204=LINE('',#10367,#1666);
#1205=LINE('',#10373,#1667);
#1206=LINE('',#10376,#1668);
#1207=LINE('',#10382,#1669);
#1208=LINE('',#10385,#1670);
#1209=LINE('',#10391,#1671);
#1210=LINE('',#10394,#1672);
#1211=LINE('',#10400,#1673);
#1212=LINE('',#10403,#1674);
#1213=LINE('',#10409,#1675);
#1214=LINE('',#10412,#1676);
#1215=LINE('',#10418,#1677);
#1216=LINE('',#10421,#1678);
#1217=LINE('',#10427,#1679);
#1218=LINE('',#10430,#1680);
#1219=LINE('',#10436,#1681);
#1220=LINE('',#10439,#1682);
#1221=LINE('',#10445,#1683);
#1222=LINE('',#10448,#1684);
#1223=LINE('',#10454,#1685);
#1224=LINE('',#10457,#1686);
#1225=LINE('',#10463,#1687);
#1226=LINE('',#10466,#1688);
#1227=LINE('',#10472,#1689);
#1228=LINE('',#10475,#1690);
#1229=LINE('',#10481,#1691);
#1230=LINE('',#10484,#1692);
#1231=LINE('',#10490,#1693);
#1232=LINE('',#10493,#1694);
#1233=LINE('',#10499,#1695);
#1234=LINE('',#10502,#1696);
#1235=LINE('',#10508,#1697);
#1236=LINE('',#10511,#1698);
#1237=LINE('',#10517,#1699);
#1238=LINE('',#10520,#1700);
#1239=LINE('',#10526,#1701);
#1240=LINE('',#10529,#1702);
#1241=LINE('',#10535,#1703);
#1242=LINE('',#10538,#1704);
#1243=LINE('',#10544,#1705);
#1244=LINE('',#10547,#1706);
#1245=LINE('',#10553,#1707);
#1246=LINE('',#10556,#1708);
#1247=LINE('',#10562,#1709);
#1248=LINE('',#10565,#1710);
#1249=LINE('',#10571,#1711);
#1250=LINE('',#10574,#1712);
#1251=LINE('',#10580,#1713);
#1252=LINE('',#10583,#1714);
#1253=LINE('',#10588,#1715);
#1254=LINE('',#10594,#1716);
#1255=LINE('',#10600,#1717);
#1256=LINE('',#10607,#1718);
#1257=LINE('',#10610,#1719);
#1258=LINE('',#10616,#1720);
#1259=LINE('',#10619,#1721);
#1260=LINE('',#10625,#1722);
#1261=LINE('',#10628,#1723);
#1262=LINE('',#10634,#1724);
#1263=LINE('',#10637,#1725);
#1264=LINE('',#10643,#1726);
#1265=LINE('',#10646,#1727);
#1266=LINE('',#10652,#1728);
#1267=LINE('',#10655,#1729);
#1268=LINE('',#10661,#1730);
#1269=LINE('',#10664,#1731);
#1270=LINE('',#10670,#1732);
#1271=LINE('',#10673,#1733);
#1272=LINE('',#10679,#1734);
#1273=LINE('',#10682,#1735);
#1274=LINE('',#10688,#1736);
#1275=LINE('',#10691,#1737);
#1276=LINE('',#10697,#1738);
#1277=LINE('',#10700,#1739);
#1278=LINE('',#10706,#1740);
#1279=LINE('',#10709,#1741);
#1280=LINE('',#10938,#1742);
#1281=LINE('',#10940,#1743);
#1282=LINE('',#10941,#1744);
#1283=LINE('',#11170,#1745);
#1284=LINE('',#11172,#1746);
#1285=LINE('',#11173,#1747);
#1286=LINE('',#11175,#1748);
#1287=LINE('',#11177,#1749);
#1288=LINE('',#11179,#1750);
#1289=LINE('',#11181,#1751);
#1290=LINE('',#11182,#1752);
#1291=LINE('',#11186,#1753);
#1292=LINE('',#11188,#1754);
#1293=LINE('',#11190,#1755);
#1294=LINE('',#11192,#1756);
#1295=LINE('',#11196,#1757);
#1296=LINE('',#11198,#1758);
#1297=LINE('',#11202,#1759);
#1298=LINE('',#11204,#1760);
#1299=LINE('',#11208,#1761);
#1300=LINE('',#11210,#1762);
#1301=LINE('',#11214,#1763);
#1302=LINE('',#11216,#1764);
#1303=LINE('',#11220,#1765);
#1304=LINE('',#11222,#1766);
#1305=LINE('',#11225,#1767);
#1306=LINE('',#11228,#1768);
#1307=LINE('',#11231,#1769);
#1308=LINE('',#11234,#1770);
#1309=LINE('',#11237,#1771);
#1310=LINE('',#11240,#1772);
#1311=LINE('',#11243,#1773);
#1312=LINE('',#11246,#1774);
#1313=LINE('',#11249,#1775);
#1314=LINE('',#11252,#1776);
#1315=LINE('',#11255,#1777);
#1316=LINE('',#11257,#1778);
#1317=LINE('',#11260,#1779);
#1318=LINE('',#11262,#1780);
#1319=LINE('',#11265,#1781);
#1320=LINE('',#11267,#1782);
#1321=LINE('',#11270,#1783);
#1322=LINE('',#11272,#1784);
#1323=LINE('',#11275,#1785);
#1324=LINE('',#11277,#1786);
#1325=LINE('',#11279,#1787);
#1326=LINE('',#11281,#1788);
#1327=LINE('',#11284,#1789);
#1328=LINE('',#11286,#1790);
#1329=LINE('',#11288,#1791);
#1330=LINE('',#11290,#1792);
#1331=LINE('',#11293,#1793);
#1332=LINE('',#11295,#1794);
#1333=LINE('',#11297,#1795);
#1334=LINE('',#11299,#1796);
#1335=LINE('',#11302,#1797);
#1336=LINE('',#11304,#1798);
#1337=LINE('',#11306,#1799);
#1338=LINE('',#11308,#1800);
#1339=LINE('',#11311,#1801);
#1340=LINE('',#11313,#1802);
#1341=LINE('',#11315,#1803);
#1342=LINE('',#11317,#1804);
#1343=LINE('',#11320,#1805);
#1344=LINE('',#11322,#1806);
#1345=LINE('',#11324,#1807);
#1346=LINE('',#11326,#1808);
#1347=LINE('',#11329,#1809);
#1348=LINE('',#11331,#1810);
#1349=LINE('',#11333,#1811);
#1350=LINE('',#11335,#1812);
#1351=LINE('',#11338,#1813);
#1352=LINE('',#11340,#1814);
#1353=LINE('',#11342,#1815);
#1354=LINE('',#11344,#1816);
#1355=LINE('',#11347,#1817);
#1356=LINE('',#11349,#1818);
#1357=LINE('',#11351,#1819);
#1358=LINE('',#11353,#1820);
#1359=LINE('',#11356,#1821);
#1360=LINE('',#11358,#1822);
#1361=LINE('',#11360,#1823);
#1362=LINE('',#11362,#1824);
#1363=LINE('',#11365,#1825);
#1364=LINE('',#11367,#1826);
#1365=LINE('',#11369,#1827);
#1366=LINE('',#11371,#1828);
#1367=LINE('',#11374,#1829);
#1368=LINE('',#11376,#1830);
#1369=LINE('',#11378,#1831);
#1370=LINE('',#11380,#1832);
#1371=LINE('',#11383,#1833);
#1372=LINE('',#11385,#1834);
#1373=LINE('',#11387,#1835);
#1374=LINE('',#11389,#1836);
#1375=LINE('',#11392,#1837);
#1376=LINE('',#11394,#1838);
#1377=LINE('',#11396,#1839);
#1378=LINE('',#11398,#1840);
#1379=LINE('',#11401,#1841);
#1380=LINE('',#11403,#1842);
#1381=LINE('',#11410,#1843);
#1382=LINE('',#11417,#1844);
#1383=LINE('',#11421,#1845);
#1384=LINE('',#11425,#1846);
#1385=LINE('',#11428,#1847);
#1386=LINE('',#11433,#1848);
#1387=LINE('',#11438,#1849);
#1388=LINE('',#11440,#1850);
#1389=LINE('',#11442,#1851);
#1390=LINE('',#11444,#1852);
#1391=LINE('',#11445,#1853);
#1392=LINE('',#11447,#1854);
#1393=LINE('',#11453,#1855);
#1394=LINE('',#11454,#1856);
#1395=LINE('',#11457,#1857);
#1396=LINE('',#11459,#1858);
#1397=LINE('',#11461,#1859);
#1398=LINE('',#11463,#1860);
#1399=LINE('',#11464,#1861);
#1400=LINE('',#11468,#1862);
#1401=LINE('',#11470,#1863);
#1402=LINE('',#11472,#1864);
#1403=LINE('',#11474,#1865);
#1404=LINE('',#11479,#1866);
#1405=LINE('',#11481,#1867);
#1406=LINE('',#11483,#1868);
#1407=LINE('',#11484,#1869);
#1408=LINE('',#11488,#1870);
#1409=LINE('',#11489,#1871);
#1410=LINE('',#11491,#1872);
#1411=LINE('',#11493,#1873);
#1412=LINE('',#11494,#1874);
#1413=LINE('',#11496,#1875);
#1414=LINE('',#11498,#1876);
#1415=LINE('',#11500,#1877);
#1416=LINE('',#11502,#1878);
#1417=LINE('',#11504,#1879);
#1418=LINE('',#11506,#1880);
#1419=LINE('',#11507,#1881);
#1420=LINE('',#11509,#1882);
#1421=LINE('',#11512,#1883);
#1422=LINE('',#11514,#1884);
#1423=LINE('',#11516,#1885);
#1424=LINE('',#11518,#1886);
#1425=LINE('',#11519,#1887);
#1426=LINE('',#11522,#1888);
#1427=LINE('',#11524,#1889);
#1428=LINE('',#11525,#1890);
#1429=LINE('',#11527,#1891);
#1430=LINE('',#11529,#1892);
#1431=LINE('',#11530,#1893);
#1432=LINE('',#11532,#1894);
#1433=LINE('',#11533,#1895);
#1434=LINE('',#11534,#1896);
#1435=LINE('',#11535,#1897);
#1436=LINE('',#11540,#1898);
#1437=LINE('',#11543,#1899);
#1438=LINE('',#11551,#1900);
#1439=LINE('',#11555,#1901);
#1440=LINE('',#11559,#1902);
#1441=LINE('',#11563,#1903);
#1442=LINE('',#11567,#1904);
#1443=LINE('',#11573,#1905);
#1444=LINE('',#11577,#1906);
#1445=LINE('',#11580,#1907);
#1446=LINE('',#11583,#1908);
#1447=LINE('',#11586,#1909);
#1448=LINE('',#11593,#1910);
#1449=LINE('',#11596,#1911);
#1450=LINE('',#11601,#1912);
#1451=LINE('',#11602,#1913);
#1452=LINE('',#11605,#1914);
#1453=LINE('',#11606,#1915);
#1454=LINE('',#11610,#1916);
#1455=LINE('',#11612,#1917);
#1456=LINE('',#11618,#1918);
#1457=LINE('',#11619,#1919);
#1458=LINE('',#11624,#1920);
#1459=LINE('',#11625,#1921);
#1460=LINE('',#11627,#1922);
#1461=LINE('',#11628,#1923);
#1462=LINE('',#11629,#1924);
#1463=LINE('',#11630,#1925);
#1464=LINE('',#11641,#1926);
#1465=LINE('',#11644,#1927);
#1466=LINE('',#11650,#1928);
#1467=LINE('',#11653,#1929);
#1468=LINE('',#11658,#1930);
#1469=LINE('',#11664,#1931);
#1470=LINE('',#11671,#1932);
#1471=LINE('',#11674,#1933);
#1472=LINE('',#11677,#1934);
#1473=LINE('',#11680,#1935);
#1474=LINE('',#11684,#1936);
#1475=LINE('',#11685,#1937);
#1476=LINE('',#11688,#1938);
#1477=LINE('',#11689,#1939);
#1478=LINE('',#11692,#1940);
#1479=LINE('',#11693,#1941);
#1480=LINE('',#11698,#1942);
#1481=LINE('',#11701,#1943);
#1482=LINE('',#11704,#1944);
#1483=LINE('',#11705,#1945);
#1484=LINE('',#11709,#1946);
#1485=LINE('',#11711,#1947);
#1486=LINE('',#11715,#1948);
#1487=LINE('',#11718,#1949);
#1488=LINE('',#11720,#1950);
#1489=LINE('',#11722,#1951);
#1490=LINE('',#11729,#1952);
#1491=LINE('',#11733,#1953);
#1492=LINE('',#11737,#1954);
#1493=LINE('',#11741,#1955);
#1494=LINE('',#11745,#1956);
#1495=LINE('',#11751,#1957);
#1496=LINE('',#11755,#1958);
#1497=LINE('',#11758,#1959);
#1498=LINE('',#11761,#1960);
#1499=LINE('',#11764,#1961);
#1500=LINE('',#11770,#1962);
#1501=LINE('',#11771,#1963);
#1502=LINE('',#11776,#1964);
#1503=LINE('',#11777,#1965);
#1504=LINE('',#11779,#1966);
#1505=LINE('',#11780,#1967);
#1506=LINE('',#11781,#1968);
#1507=LINE('',#11782,#1969);
#1508=LINE('',#11792,#1970);
#1509=LINE('',#11795,#1971);
#1510=LINE('',#11798,#1972);
#1511=LINE('',#11801,#1973);
#1512=LINE('',#11804,#1974);
#1513=LINE('',#11805,#1975);
#1514=LINE('',#11808,#1976);
#1515=LINE('',#11811,#1977);
#1516=LINE('',#11827,#1978);
#1517=LINE('',#11830,#1979);
#1518=LINE('',#11833,#1980);
#1519=LINE('',#11840,#1981);
#1520=LINE('',#11844,#1982);
#1521=LINE('',#11849,#1983);
#1522=LINE('',#11853,#1984);
#1523=LINE('',#11856,#1985);
#1524=LINE('',#11859,#1986);
#1525=LINE('',#11862,#1987);
#1526=LINE('',#11864,#1988);
#1527=LINE('',#11865,#1989);
#1528=LINE('',#11868,#1990);
#1529=LINE('',#11871,#1991);
#1530=LINE('',#11872,#1992);
#1531=LINE('',#11873,#1993);
#1532=LINE('',#11875,#1994);
#1533=LINE('',#11876,#1995);
#1534=VECTOR('',#7658,1.5);
#1535=VECTOR('',#7665,1.5);
#1536=VECTOR('',#7672,1.5);
#1537=VECTOR('',#7679,1.5);
#1538=VECTOR('',#7684,1000.);
#1539=VECTOR('',#7685,1000.);
#1540=VECTOR('',#7686,1000.);
#1541=VECTOR('',#7687,1000.);
#1542=VECTOR('',#7690,1000.);
#1543=VECTOR('',#7691,1000.);
#1544=VECTOR('',#7692,1000.);
#1545=VECTOR('',#7695,1000.);
#1546=VECTOR('',#7696,1000.);
#1547=VECTOR('',#7697,1000.);
#1548=VECTOR('',#7700,1000.);
#1549=VECTOR('',#7701,1000.);
#1550=VECTOR('',#7702,1000.);
#1551=VECTOR('',#7705,1000.);
#1552=VECTOR('',#7706,1000.);
#1553=VECTOR('',#7707,1000.);
#1554=VECTOR('',#7708,1000.);
#1555=VECTOR('',#7713,1000.);
#1556=VECTOR('',#7716,1000.);
#1557=VECTOR('',#7721,1000.);
#1558=VECTOR('',#7726,1000.);
#1559=VECTOR('',#7727,1000.);
#1560=VECTOR('',#7728,1000.);
#1561=VECTOR('',#7733,1000.);
#1562=VECTOR('',#7736,1000.);
#1563=VECTOR('',#7741,1000.);
#1564=VECTOR('',#7748,1000.);
#1565=VECTOR('',#7753,1000.);
#1566=VECTOR('',#7754,1000.);
#1567=VECTOR('',#7755,1000.);
#1568=VECTOR('',#7764,1000.);
#1569=VECTOR('',#7765,1000.);
#1570=VECTOR('',#7788,3.);
#1571=VECTOR('',#7795,1000.);
#1572=VECTOR('',#7798,1000.);
#1573=VECTOR('',#7803,1000.);
#1574=VECTOR('',#7806,1000.);
#1575=VECTOR('',#7811,1.5);
#1576=VECTOR('',#7818,1.5);
#1577=VECTOR('',#7827,1000.);
#1578=VECTOR('',#7830,1000.);
#1579=VECTOR('',#7837,1000.);
#1580=VECTOR('',#7838,1000.);
#1581=VECTOR('',#7841,1000.);
#1582=VECTOR('',#7842,1000.);
#1583=VECTOR('',#7845,1000.);
#1584=VECTOR('',#7846,1000.);
#1585=VECTOR('',#7849,1000.);
#1586=VECTOR('',#7852,1000.);
#1587=VECTOR('',#7853,1000.);
#1588=VECTOR('',#7856,1000.);
#1589=VECTOR('',#7859,1000.);
#1590=VECTOR('',#7862,1000.);
#1591=VECTOR('',#7867,1000.);
#1592=VECTOR('',#7870,1000.);
#1593=VECTOR('',#7873,1000.);
#1594=VECTOR('',#7876,1000.);
#1595=VECTOR('',#7881,1000.);
#1596=VECTOR('',#7882,1000.);
#1597=VECTOR('',#7887,1000.);
#1598=VECTOR('',#7890,1000.);
#1599=VECTOR('',#7895,1000.);
#1600=VECTOR('',#7896,1000.);
#1601=VECTOR('',#7897,1000.);
#1602=VECTOR('',#7900,1000.);
#1603=VECTOR('',#7901,1000.);
#1604=VECTOR('',#7902,1000.);
#1605=VECTOR('',#7905,1000.);
#1606=VECTOR('',#7910,1000.);
#1607=VECTOR('',#7911,1000.);
#1608=VECTOR('',#7914,1000.);
#1609=VECTOR('',#7925,1.5);
#1610=VECTOR('',#7932,1000.);
#1611=VECTOR('',#7935,1000.);
#1612=VECTOR('',#7940,3.);
#1613=VECTOR('',#7947,1000.);
#1614=VECTOR('',#7950,1000.);
#1615=VECTOR('',#7955,1000.);
#1616=VECTOR('',#7958,1000.);
#1617=VECTOR('',#7963,1.5);
#1618=VECTOR('',#7970,1.5);
#1619=VECTOR('',#7975,1000.);
#1620=VECTOR('',#7976,1000.);
#1621=VECTOR('',#7977,1000.);
#1622=VECTOR('',#7982,1000.);
#1623=VECTOR('',#7983,1000.);
#1624=VECTOR('',#7984,1000.);
#1625=VECTOR('',#7987,1000.);
#1626=VECTOR('',#7988,1000.);
#1627=VECTOR('',#7989,1000.);
#1628=VECTOR('',#7992,1000.);
#1629=VECTOR('',#7993,1000.);
#1630=VECTOR('',#7996,1000.);
#1631=VECTOR('',#7997,1000.);
#1632=VECTOR('',#8000,1000.);
#1633=VECTOR('',#8003,1000.);
#1634=VECTOR('',#8006,1000.);
#1635=VECTOR('',#8007,1000.);
#1636=VECTOR('',#8010,1000.);
#1637=VECTOR('',#8013,1000.);
#1638=VECTOR('',#8016,1000.);
#1639=VECTOR('',#8019,1000.);
#1640=VECTOR('',#8022,1000.);
#1641=VECTOR('',#8025,1000.);
#1642=VECTOR('',#8030,1000.);
#1643=VECTOR('',#8031,1000.);
#1644=VECTOR('',#8036,1000.);
#1645=VECTOR('',#8039,1000.);
#1646=VECTOR('',#8044,1000.);
#1647=VECTOR('',#8045,1000.);
#1648=VECTOR('',#8046,1000.);
#1649=VECTOR('',#8049,1000.);
#1650=VECTOR('',#8054,1000.);
#1651=VECTOR('',#8055,1000.);
#1652=VECTOR('',#8058,1000.);
#1653=VECTOR('',#8069,1000.);
#1654=VECTOR('',#8072,1000.);
#1655=VECTOR('',#8077,1000.);
#1656=VECTOR('',#8080,1000.);
#1657=VECTOR('',#8085,1000.);
#1658=VECTOR('',#8092,1000.);
#1659=VECTOR('',#8095,1000.);
#1660=VECTOR('',#8100,1000.);
#1661=VECTOR('',#8107,1000.);
#1662=VECTOR('',#8110,1000.);
#1663=VECTOR('',#8117,1000.);
#1664=VECTOR('',#8122,1000.);
#1665=VECTOR('',#8125,1000.);
#1666=VECTOR('',#8132,1000.);
#1667=VECTOR('',#8137,1000.);
#1668=VECTOR('',#8140,1000.);
#1669=VECTOR('',#8145,1000.);
#1670=VECTOR('',#8148,1000.);
#1671=VECTOR('',#8153,1000.);
#1672=VECTOR('',#8156,1000.);
#1673=VECTOR('',#8161,1000.);
#1674=VECTOR('',#8164,1000.);
#1675=VECTOR('',#8169,1000.);
#1676=VECTOR('',#8172,1000.);
#1677=VECTOR('',#8177,1000.);
#1678=VECTOR('',#8180,1000.);
#1679=VECTOR('',#8185,1000.);
#1680=VECTOR('',#8188,1000.);
#1681=VECTOR('',#8193,1000.);
#1682=VECTOR('',#8196,1000.);
#1683=VECTOR('',#8201,1000.);
#1684=VECTOR('',#8204,1000.);
#1685=VECTOR('',#8209,1000.);
#1686=VECTOR('',#8212,1000.);
#1687=VECTOR('',#8217,1000.);
#1688=VECTOR('',#8220,1000.);
#1689=VECTOR('',#8225,1000.);
#1690=VECTOR('',#8228,1000.);
#1691=VECTOR('',#8233,1000.);
#1692=VECTOR('',#8236,1000.);
#1693=VECTOR('',#8241,1000.);
#1694=VECTOR('',#8244,1000.);
#1695=VECTOR('',#8249,1000.);
#1696=VECTOR('',#8252,1000.);
#1697=VECTOR('',#8257,1000.);
#1698=VECTOR('',#8260,1000.);
#1699=VECTOR('',#8265,1000.);
#1700=VECTOR('',#8268,1000.);
#1701=VECTOR('',#8273,1000.);
#1702=VECTOR('',#8276,1000.);
#1703=VECTOR('',#8281,1000.);
#1704=VECTOR('',#8284,1000.);
#1705=VECTOR('',#8289,1000.);
#1706=VECTOR('',#8292,1000.);
#1707=VECTOR('',#8297,1000.);
#1708=VECTOR('',#8300,1000.);
#1709=VECTOR('',#8305,1000.);
#1710=VECTOR('',#8308,1000.);
#1711=VECTOR('',#8313,1000.);
#1712=VECTOR('',#8316,1000.);
#1713=VECTOR('',#8321,1000.);
#1714=VECTOR('',#8324,1000.);
#1715=VECTOR('',#8329,1000.);
#1716=VECTOR('',#8336,1000.);
#1717=VECTOR('',#8343,1000.);
#1718=VECTOR('',#8350,1000.);
#1719=VECTOR('',#8353,1000.);
#1720=VECTOR('',#8358,1000.);
#1721=VECTOR('',#8361,1000.);
#1722=VECTOR('',#8366,1000.);
#1723=VECTOR('',#8369,1000.);
#1724=VECTOR('',#8374,1000.);
#1725=VECTOR('',#8377,1000.);
#1726=VECTOR('',#8382,1000.);
#1727=VECTOR('',#8385,1000.);
#1728=VECTOR('',#8390,1000.);
#1729=VECTOR('',#8393,1000.);
#1730=VECTOR('',#8398,1000.);
#1731=VECTOR('',#8401,1000.);
#1732=VECTOR('',#8406,1000.);
#1733=VECTOR('',#8409,1000.);
#1734=VECTOR('',#8414,1000.);
#1735=VECTOR('',#8417,1000.);
#1736=VECTOR('',#8422,1000.);
#1737=VECTOR('',#8425,1000.);
#1738=VECTOR('',#8430,1000.);
#1739=VECTOR('',#8433,1000.);
#1740=VECTOR('',#8438,1000.);
#1741=VECTOR('',#8441,1000.);
#1742=VECTOR('',#8710,1000.);
#1743=VECTOR('',#8711,1000.);
#1744=VECTOR('',#8712,1000.);
#1745=VECTOR('',#8981,1000.);
#1746=VECTOR('',#8982,1000.);
#1747=VECTOR('',#8983,1000.);
#1748=VECTOR('',#8986,1000.);
#1749=VECTOR('',#8989,1000.);
#1750=VECTOR('',#8992,1000.);
#1751=VECTOR('',#8995,1000.);
#1752=VECTOR('',#8996,1000.);
#1753=VECTOR('',#9003,1000.);
#1754=VECTOR('',#9006,1000.);
#1755=VECTOR('',#9009,1000.);
#1756=VECTOR('',#9012,1000.);
#1757=VECTOR('',#9019,1000.);
#1758=VECTOR('',#9022,1000.);
#1759=VECTOR('',#9029,1000.);
#1760=VECTOR('',#9032,1000.);
#1761=VECTOR('',#9039,1000.);
#1762=VECTOR('',#9042,1000.);
#1763=VECTOR('',#9049,1000.);
#1764=VECTOR('',#9052,1000.);
#1765=VECTOR('',#9059,1000.);
#1766=VECTOR('',#9062,1000.);
#1767=VECTOR('',#9067,1000.);
#1768=VECTOR('',#9072,1000.);
#1769=VECTOR('',#9077,1000.);
#1770=VECTOR('',#9082,1000.);
#1771=VECTOR('',#9087,1000.);
#1772=VECTOR('',#9092,1000.);
#1773=VECTOR('',#9097,1000.);
#1774=VECTOR('',#9102,1000.);
#1775=VECTOR('',#9107,1000.);
#1776=VECTOR('',#9112,1000.);
#1777=VECTOR('',#9117,1000.);
#1778=VECTOR('',#9120,1000.);
#1779=VECTOR('',#9125,1000.);
#1780=VECTOR('',#9128,1000.);
#1781=VECTOR('',#9133,1000.);
#1782=VECTOR('',#9136,1000.);
#1783=VECTOR('',#9141,1000.);
#1784=VECTOR('',#9144,1000.);
#1785=VECTOR('',#9149,1000.);
#1786=VECTOR('',#9152,1000.);
#1787=VECTOR('',#9155,1000.);
#1788=VECTOR('',#9158,1000.);
#1789=VECTOR('',#9163,1000.);
#1790=VECTOR('',#9166,1000.);
#1791=VECTOR('',#9169,1000.);
#1792=VECTOR('',#9172,1000.);
#1793=VECTOR('',#9177,1000.);
#1794=VECTOR('',#9180,1000.);
#1795=VECTOR('',#9183,1000.);
#1796=VECTOR('',#9186,1000.);
#1797=VECTOR('',#9191,1000.);
#1798=VECTOR('',#9194,1000.);
#1799=VECTOR('',#9197,1000.);
#1800=VECTOR('',#9200,1000.);
#1801=VECTOR('',#9205,1000.);
#1802=VECTOR('',#9208,1000.);
#1803=VECTOR('',#9211,1000.);
#1804=VECTOR('',#9214,1000.);
#1805=VECTOR('',#9219,1000.);
#1806=VECTOR('',#9222,1000.);
#1807=VECTOR('',#9225,1000.);
#1808=VECTOR('',#9228,1000.);
#1809=VECTOR('',#9233,1000.);
#1810=VECTOR('',#9236,1000.);
#1811=VECTOR('',#9239,1000.);
#1812=VECTOR('',#9242,1000.);
#1813=VECTOR('',#9247,1000.);
#1814=VECTOR('',#9250,1000.);
#1815=VECTOR('',#9253,1000.);
#1816=VECTOR('',#9256,1000.);
#1817=VECTOR('',#9261,1000.);
#1818=VECTOR('',#9264,1000.);
#1819=VECTOR('',#9267,1000.);
#1820=VECTOR('',#9270,1000.);
#1821=VECTOR('',#9275,1000.);
#1822=VECTOR('',#9278,1000.);
#1823=VECTOR('',#9281,1000.);
#1824=VECTOR('',#9284,1000.);
#1825=VECTOR('',#9289,1000.);
#1826=VECTOR('',#9292,1000.);
#1827=VECTOR('',#9295,1000.);
#1828=VECTOR('',#9298,1000.);
#1829=VECTOR('',#9303,1000.);
#1830=VECTOR('',#9306,1000.);
#1831=VECTOR('',#9309,1000.);
#1832=VECTOR('',#9312,1000.);
#1833=VECTOR('',#9317,1000.);
#1834=VECTOR('',#9320,1000.);
#1835=VECTOR('',#9323,1000.);
#1836=VECTOR('',#9326,1000.);
#1837=VECTOR('',#9331,1000.);
#1838=VECTOR('',#9334,1000.);
#1839=VECTOR('',#9337,1000.);
#1840=VECTOR('',#9340,1000.);
#1841=VECTOR('',#9345,1000.);
#1842=VECTOR('',#9348,1000.);
#1843=VECTOR('',#9357,1.5);
#1844=VECTOR('',#9364,1000.);
#1845=VECTOR('',#9367,1000.);
#1846=VECTOR('',#9370,1000.);
#1847=VECTOR('',#9373,1000.);
#1848=VECTOR('',#9378,1.5);
#1849=VECTOR('',#9383,1000.);
#1850=VECTOR('',#9384,1000.);
#1851=VECTOR('',#9385,1000.);
#1852=VECTOR('',#9386,1000.);
#1853=VECTOR('',#9387,1000.);
#1854=VECTOR('',#9388,1000.);
#1855=VECTOR('',#9393,1000.);
#1856=VECTOR('',#9394,1000.);
#1857=VECTOR('',#9397,1000.);
#1858=VECTOR('',#9398,1000.);
#1859=VECTOR('',#9399,1000.);
#1860=VECTOR('',#9400,1000.);
#1861=VECTOR('',#9401,1000.);
#1862=VECTOR('',#9404,1000.);
#1863=VECTOR('',#9405,1000.);
#1864=VECTOR('',#9406,1000.);
#1865=VECTOR('',#9407,1000.);
#1866=VECTOR('',#9412,1000.);
#1867=VECTOR('',#9413,1000.);
#1868=VECTOR('',#9414,1000.);
#1869=VECTOR('',#9415,1000.);
#1870=VECTOR('',#9418,1000.);
#1871=VECTOR('',#9419,1000.);
#1872=VECTOR('',#9420,1000.);
#1873=VECTOR('',#9421,1000.);
#1874=VECTOR('',#9422,1000.);
#1875=VECTOR('',#9425,1000.);
#1876=VECTOR('',#9428,1000.);
#1877=VECTOR('',#9431,1000.);
#1878=VECTOR('',#9434,1000.);
#1879=VECTOR('',#9437,1000.);
#1880=VECTOR('',#9440,1000.);
#1881=VECTOR('',#9441,1000.);
#1882=VECTOR('',#9444,1000.);
#1883=VECTOR('',#9447,1000.);
#1884=VECTOR('',#9448,1000.);
#1885=VECTOR('',#9449,1000.);
#1886=VECTOR('',#9450,1000.);
#1887=VECTOR('',#9451,1000.);
#1888=VECTOR('',#9454,1000.);
#1889=VECTOR('',#9455,1000.);
#1890=VECTOR('',#9456,1000.);
#1891=VECTOR('',#9459,1000.);
#1892=VECTOR('',#9460,1000.);
#1893=VECTOR('',#9461,1000.);
#1894=VECTOR('',#9462,1000.);
#1895=VECTOR('',#9463,1000.);
#1896=VECTOR('',#9464,1000.);
#1897=VECTOR('',#9465,1000.);
#1898=VECTOR('',#9474,1000.);
#1899=VECTOR('',#9479,1000.);
#1900=VECTOR('',#9490,1.25);
#1901=VECTOR('',#9493,1000.);
#1902=VECTOR('',#9496,1000.);
#1903=VECTOR('',#9499,1000.);
#1904=VECTOR('',#9502,1000.);
#1905=VECTOR('',#9509,1.5);
#1906=VECTOR('',#9514,1000.);
#1907=VECTOR('',#9517,1000.);
#1908=VECTOR('',#9520,1000.);
#1909=VECTOR('',#9523,1000.);
#1910=VECTOR('',#9530,1000.);
#1911=VECTOR('',#9533,1000.);
#1912=VECTOR('',#9538,1000.);
#1913=VECTOR('',#9539,1000.);
#1914=VECTOR('',#9542,1000.);
#1915=VECTOR('',#9543,1000.);
#1916=VECTOR('',#9548,1000.);
#1917=VECTOR('',#9551,1000.);
#1918=VECTOR('',#9558,1000.);
#1919=VECTOR('',#9559,1000.);
#1920=VECTOR('',#9564,1000.);
#1921=VECTOR('',#9565,1000.);
#1922=VECTOR('',#9568,1000.);
#1923=VECTOR('',#9569,1000.);
#1924=VECTOR('',#9570,1000.);
#1925=VECTOR('',#9571,1000.);
#1926=VECTOR('',#9586,1000.);
#1927=VECTOR('',#9589,1000.);
#1928=VECTOR('',#9594,1000.);
#1929=VECTOR('',#9597,1000.);
#1930=VECTOR('',#9602,1.5);
#1931=VECTOR('',#9609,1.5);
#1932=VECTOR('',#9616,1000.);
#1933=VECTOR('',#9619,1000.);
#1934=VECTOR('',#9622,1000.);
#1935=VECTOR('',#9625,1000.);
#1936=VECTOR('',#9628,1000.);
#1937=VECTOR('',#9629,1000.);
#1938=VECTOR('',#9632,1000.);
#1939=VECTOR('',#9633,1000.);
#1940=VECTOR('',#9636,1000.);
#1941=VECTOR('',#9637,1000.);
#1942=VECTOR('',#9644,1000.);
#1943=VECTOR('',#9647,1000.);
#1944=VECTOR('',#9650,1000.);
#1945=VECTOR('',#9651,1000.);
#1946=VECTOR('',#9656,1000.);
#1947=VECTOR('',#9659,1000.);
#1948=VECTOR('',#9664,1000.);
#1949=VECTOR('',#9667,1000.);
#1950=VECTOR('',#9670,1000.);
#1951=VECTOR('',#9673,1000.);
#1952=VECTOR('',#9682,1.25);
#1953=VECTOR('',#9685,1000.);
#1954=VECTOR('',#9688,1000.);
#1955=VECTOR('',#9691,1000.);
#1956=VECTOR('',#9694,1000.);
#1957=VECTOR('',#9701,1.5);
#1958=VECTOR('',#9706,1000.);
#1959=VECTOR('',#9709,1000.);
#1960=VECTOR('',#9712,1000.);
#1961=VECTOR('',#9715,1000.);
#1962=VECTOR('',#9722,1000.);
#1963=VECTOR('',#9723,1000.);
#1964=VECTOR('',#9728,1000.);
#1965=VECTOR('',#9729,1000.);
#1966=VECTOR('',#9732,1000.);
#1967=VECTOR('',#9733,1000.);
#1968=VECTOR('',#9734,1000.);
#1969=VECTOR('',#9735,1000.);
#1970=VECTOR('',#9748,1000.);
#1971=VECTOR('',#9751,1000.);
#1972=VECTOR('',#9754,1000.);
#1973=VECTOR('',#9757,1000.);
#1974=VECTOR('',#9760,1000.);
#1975=VECTOR('',#9761,1000.);
#1976=VECTOR('',#9764,1000.);
#1977=VECTOR('',#9769,1000.);
#1978=VECTOR('',#9788,1000.);
#1979=VECTOR('',#9791,1000.);
#1980=VECTOR('',#9794,2.5);
#1981=VECTOR('',#9801,1000.);
#1982=VECTOR('',#9804,1.5);
#1983=VECTOR('',#9809,1000.);
#1984=VECTOR('',#9812,1000.);
#1985=VECTOR('',#9815,1000.);
#1986=VECTOR('',#9818,1000.);
#1987=VECTOR('',#9821,1000.);
#1988=VECTOR('',#9824,1000.);
#1989=VECTOR('',#9825,1000.);
#1990=VECTOR('',#9828,1000.);
#1991=VECTOR('',#9831,1000.);
#1992=VECTOR('',#9832,1000.);
#1993=VECTOR('',#9833,1000.);
#1994=VECTOR('',#9836,1000.);
#1995=VECTOR('',#9837,1000.);
#1996=CIRCLE('',#6755,1.5);
#1997=CIRCLE('',#6756,1.5);
#1998=CIRCLE('',#6758,1.5);
#1999=CIRCLE('',#6759,1.5);
#2000=CIRCLE('',#6761,1.5);
#2001=CIRCLE('',#6762,1.5);
#2002=CIRCLE('',#6764,1.5);
#2003=CIRCLE('',#6765,1.5);
#2004=CIRCLE('',#6772,14.);
#2005=CIRCLE('',#6773,14.);
#2006=CIRCLE('',#6775,5.);
#2007=CIRCLE('',#6776,5.);
#2008=CIRCLE('',#6779,5.);
#2009=CIRCLE('',#6780,5.);
#2010=CIRCLE('',#6782,14.);
#2011=CIRCLE('',#6783,14.);
#2012=CIRCLE('',#6785,5.);
#2013=CIRCLE('',#6786,5.);
#2014=CIRCLE('',#6789,5.);
#2015=CIRCLE('',#6790,5.);
#2016=CIRCLE('',#6793,12.);
#2017=CIRCLE('',#6794,12.);
#2018=CIRCLE('',#6796,12.);
#2019=CIRCLE('',#6797,12.);
#2020=CIRCLE('',#6802,3.);
#2021=CIRCLE('',#6803,3.);
#2022=CIRCLE('',#6805,3.5);
#2023=CIRCLE('',#6806,3.5);
#2024=CIRCLE('',#6808,3.5);
#2025=CIRCLE('',#6809,3.5);
#2026=CIRCLE('',#6811,1.5);
#2027=CIRCLE('',#6812,1.5);
#2028=CIRCLE('',#6814,1.5);
#2029=CIRCLE('',#6815,1.5);
#2030=CIRCLE('',#6817,3.5);
#2031=CIRCLE('',#6818,3.5);
#2032=CIRCLE('',#6819,3.5);
#2033=CIRCLE('',#6820,3.5);
#2034=CIRCLE('',#6822,3.);
#2035=CIRCLE('',#6823,3.5);
#2036=CIRCLE('',#6824,3.5);
#2037=CIRCLE('',#6826,3.5);
#2038=CIRCLE('',#6827,3.5);
#2039=CIRCLE('',#6832,3.5);
#2040=CIRCLE('',#6838,3.5);
#2041=CIRCLE('',#6844,3.);
#2042=CIRCLE('',#6851,1.5);
#2043=CIRCLE('',#6852,1.5);
#2044=CIRCLE('',#6854,3.5);
#2045=CIRCLE('',#6855,3.5);
#2046=CIRCLE('',#6857,3.);
#2047=CIRCLE('',#6858,3.);
#2048=CIRCLE('',#6860,3.5);
#2049=CIRCLE('',#6861,3.5);
#2050=CIRCLE('',#6863,3.5);
#2051=CIRCLE('',#6864,3.5);
#2052=CIRCLE('',#6866,1.5);
#2053=CIRCLE('',#6867,1.5);
#2054=CIRCLE('',#6869,1.5);
#2055=CIRCLE('',#6870,1.5);
#2056=CIRCLE('',#6873,3.);
#2057=CIRCLE('',#6874,3.5);
#2058=CIRCLE('',#6875,3.5);
#2059=CIRCLE('',#6877,3.5);
#2060=CIRCLE('',#6878,3.5);
#2061=CIRCLE('',#6883,3.5);
#2062=CIRCLE('',#6889,3.5);
#2063=CIRCLE('',#6894,3.);
#2064=CIRCLE('',#6901,3.);
#2065=CIRCLE('',#6902,3.);
#2066=CIRCLE('',#6904,0.269999999999999);
#2067=CIRCLE('',#6905,0.269999999999999);
#2068=CIRCLE('',#6907,3.68751484013274);
#2069=CIRCLE('',#6908,3.68751484013273);
#2070=CIRCLE('',#6910,0.269999999999999);
#2071=CIRCLE('',#6911,0.269999999999999);
#2072=CIRCLE('',#6913,3.68751484013275);
#2073=CIRCLE('',#6914,3.68751484013275);
#2074=CIRCLE('',#6916,0.269999999999996);
#2075=CIRCLE('',#6917,0.269999999999996);
#2076=CIRCLE('',#6919,3.68751484013273);
#2077=CIRCLE('',#6920,3.68751484013274);
#2078=CIRCLE('',#6922,0.27);
#2079=CIRCLE('',#6923,0.27);
#2080=CIRCLE('',#6925,3.68751484013274);
#2081=CIRCLE('',#6926,3.68751484013274);
#2082=CIRCLE('',#6928,0.269999999999999);
#2083=CIRCLE('',#6929,0.269999999999999);
#2084=CIRCLE('',#6931,0.269999999999999);
#2085=CIRCLE('',#6932,0.269999999999999);
#2086=CIRCLE('',#6934,0.270000000000005);
#2087=CIRCLE('',#6935,0.270000000000005);
#2088=CIRCLE('',#6937,0.269999999999999);
#2089=CIRCLE('',#6938,0.269999999999999);
#2090=CIRCLE('',#6940,0.269999999999999);
#2091=CIRCLE('',#6941,0.269999999999999);
#2092=CIRCLE('',#6943,0.269999999999999);
#2093=CIRCLE('',#6944,0.269999999999999);
#2094=CIRCLE('',#6946,0.269999999999999);
#2095=CIRCLE('',#6947,0.269999999999999);
#2096=CIRCLE('',#6949,0.269999999999999);
#2097=CIRCLE('',#6950,0.269999999999999);
#2098=CIRCLE('',#6952,0.269999999999999);
#2099=CIRCLE('',#6953,0.269999999999999);
#2100=CIRCLE('',#6955,0.270000000000003);
#2101=CIRCLE('',#6956,0.270000000000003);
#2102=CIRCLE('',#6958,14.3999999999983);
#2103=CIRCLE('',#6959,14.3999999999981);
#2104=CIRCLE('',#6961,14.399999999999);
#2105=CIRCLE('',#6962,14.4000000000003);
#2106=CIRCLE('',#6964,14.4000000000038);
#2107=CIRCLE('',#6965,14.4000000000017);
#2108=CIRCLE('',#6967,14.4000000000006);
#2109=CIRCLE('',#6968,14.4000000000006);
#2110=CIRCLE('',#6970,14.3999999999975);
#2111=CIRCLE('',#6971,14.4000000000014);
#2112=CIRCLE('',#6973,14.399999999997);
#2113=CIRCLE('',#6974,14.399999999997);
#2114=CIRCLE('',#6976,14.4000000000003);
#2115=CIRCLE('',#6977,14.3999999999984);
#2116=CIRCLE('',#6979,14.4);
#2117=CIRCLE('',#6980,14.4000000000003);
#2118=CIRCLE('',#6982,14.4000000000016);
#2119=CIRCLE('',#6983,14.4000000000016);
#2120=CIRCLE('',#6985,14.4000000000005);
#2121=CIRCLE('',#6986,14.4000000000001);
#2122=CIRCLE('',#6988,14.3999999999991);
#2123=CIRCLE('',#6989,14.3999999999994);
#2124=CIRCLE('',#6991,14.3999999999988);
#2125=CIRCLE('',#6992,14.3999999999988);
#2126=CIRCLE('',#6994,14.4000000000015);
#2127=CIRCLE('',#6995,14.4000000000014);
#2128=CIRCLE('',#6997,14.4000000000037);
#2129=CIRCLE('',#6998,14.4000000000039);
#2130=CIRCLE('',#7000,14.4000000000005);
#2131=CIRCLE('',#7001,14.4000000000006);
#2132=CIRCLE('',#7003,14.3999999999991);
#2133=CIRCLE('',#7004,14.3999999999995);
#2134=CIRCLE('',#7006,14.4000000000014);
#2135=CIRCLE('',#7007,14.4000000000014);
#2136=CIRCLE('',#7009,14.4000000000019);
#2137=CIRCLE('',#7010,14.4000000000005);
#2138=CIRCLE('',#7012,14.4000000000007);
#2139=CIRCLE('',#7013,14.4000000000011);
#2140=CIRCLE('',#7015,14.4000000000004);
#2141=CIRCLE('',#7016,14.4000000000004);
#2142=CIRCLE('',#7018,14.3999999999997);
#2143=CIRCLE('',#7019,14.3999999999997);
#2144=CIRCLE('',#7021,14.4000000000024);
#2145=CIRCLE('',#7022,14.4000000000024);
#2146=CIRCLE('',#7024,14.3999999999984);
#2147=CIRCLE('',#7025,14.3999999999984);
#2148=CIRCLE('',#7027,14.4000000000024);
#2149=CIRCLE('',#7028,14.4);
#2150=CIRCLE('',#7030,14.4000000000004);
#2151=CIRCLE('',#7031,14.3999999999987);
#2152=CIRCLE('',#7033,14.4000000000022);
#2153=CIRCLE('',#7034,14.4000000000021);
#2154=CIRCLE('',#7036,14.400000000003);
#2155=CIRCLE('',#7037,14.400000000002);
#2156=CIRCLE('',#7039,14.3999999999986);
#2157=CIRCLE('',#7040,14.3999999999991);
#2158=CIRCLE('',#7042,14.3999999999986);
#2159=CIRCLE('',#7043,14.3999999999986);
#2160=CIRCLE('',#7045,3.68751484013278);
#2161=CIRCLE('',#7046,0.269999999999998);
#2162=CIRCLE('',#7047,12.3749999999972);
#2163=CIRCLE('',#7048,0.270000000000001);
#2164=CIRCLE('',#7049,3.68751484013274);
#2165=CIRCLE('',#7050,3.68751484013271);
#2166=CIRCLE('',#7051,0.269999999999999);
#2167=CIRCLE('',#7052,12.3750000000014);
#2168=CIRCLE('',#7053,0.269999999999998);
#2169=CIRCLE('',#7054,3.68751484013275);
#2170=CIRCLE('',#7055,3.68751484013276);
#2171=CIRCLE('',#7056,0.270000000000001);
#2172=CIRCLE('',#7057,12.3750000000098);
#2173=CIRCLE('',#7058,0.270000000000001);
#2174=CIRCLE('',#7059,3.68751484013276);
#2175=CIRCLE('',#7060,3.68751484013274);
#2176=CIRCLE('',#7061,0.270000000000003);
#2177=CIRCLE('',#7062,12.3750000000051);
#2178=CIRCLE('',#7063,0.270000000000001);
#2179=CIRCLE('',#7064,3.68751484013274);
#2180=CIRCLE('',#7065,3.68751484013273);
#2181=CIRCLE('',#7066,0.269999999999998);
#2182=CIRCLE('',#7067,12.3749999999976);
#2183=CIRCLE('',#7068,0.269999999999999);
#2184=CIRCLE('',#7069,3.68751484013276);
#2185=CIRCLE('',#7070,3.68751484013274);
#2186=CIRCLE('',#7071,0.270000000000001);
#2187=CIRCLE('',#7072,12.3750000000045);
#2188=CIRCLE('',#7073,0.269999999999998);
#2189=CIRCLE('',#7074,3.68751484013275);
#2190=CIRCLE('',#7075,3.68751484013276);
#2191=CIRCLE('',#7076,0.269999999999999);
#2192=CIRCLE('',#7077,12.3749999999983);
#2193=CIRCLE('',#7078,0.270000000000001);
#2194=CIRCLE('',#7079,3.68751484013274);
#2195=CIRCLE('',#7080,3.68751484013275);
#2196=CIRCLE('',#7081,0.270000000000003);
#2197=CIRCLE('',#7082,12.3749999999972);
#2198=CIRCLE('',#7083,0.269999999999999);
#2199=CIRCLE('',#7084,3.68751484013273);
#2200=CIRCLE('',#7085,3.68751484013272);
#2201=CIRCLE('',#7086,0.270000000000003);
#2202=CIRCLE('',#7087,12.3750000000007);
#2203=CIRCLE('',#7088,0.270000000000001);
#2204=CIRCLE('',#7089,3.68751484013272);
#2205=CIRCLE('',#7090,3.68751484013275);
#2206=CIRCLE('',#7091,0.269999999999999);
#2207=CIRCLE('',#7092,12.3749999999991);
#2208=CIRCLE('',#7093,0.270000000000002);
#2209=CIRCLE('',#7094,3.68751484013276);
#2210=CIRCLE('',#7095,3.68751484013277);
#2211=CIRCLE('',#7096,0.27);
#2212=CIRCLE('',#7097,12.374999999999);
#2213=CIRCLE('',#7098,0.27);
#2214=CIRCLE('',#7099,3.68751484013274);
#2215=CIRCLE('',#7100,3.68751484013273);
#2216=CIRCLE('',#7101,0.270000000000002);
#2217=CIRCLE('',#7102,12.3749999999924);
#2218=CIRCLE('',#7103,0.270000000000002);
#2219=CIRCLE('',#7104,3.68751484013273);
#2220=CIRCLE('',#7105,12.3749999999951);
#2221=CIRCLE('',#7106,0.270000000000001);
#2222=CIRCLE('',#7107,3.68751484013273);
#2223=CIRCLE('',#7108,12.3750000000026);
#2224=CIRCLE('',#7109,0.269999999999999);
#2225=CIRCLE('',#7110,3.68751484013277);
#2226=CIRCLE('',#7111,3.68751484013274);
#2227=CIRCLE('',#7112,12.3750000000013);
#2228=CIRCLE('',#7113,0.269999999999999);
#2229=CIRCLE('',#7114,3.68751484013274);
#2230=CIRCLE('',#7115,3.68751484013272);
#2231=CIRCLE('',#7116,12.375);
#2232=CIRCLE('',#7117,0.269999999999999);
#2233=CIRCLE('',#7118,3.68751484013274);
#2234=CIRCLE('',#7119,3.68751484013274);
#2235=CIRCLE('',#7120,12.3750000000006);
#2236=CIRCLE('',#7121,0.269999999999999);
#2237=CIRCLE('',#7122,3.68751484013276);
#2238=CIRCLE('',#7123,3.68751484013275);
#2239=CIRCLE('',#7124,12.3749999999985);
#2240=CIRCLE('',#7125,0.270000000000001);
#2241=CIRCLE('',#7126,3.68751484013274);
#2242=CIRCLE('',#7127,3.68751484013273);
#2243=CIRCLE('',#7128,12.3750000000014);
#2244=CIRCLE('',#7129,0.270000000000001);
#2245=CIRCLE('',#7130,3.68751484013275);
#2246=CIRCLE('',#7131,3.68751484013273);
#2247=CIRCLE('',#7132,0.270000000000001);
#2248=CIRCLE('',#7133,12.3750000000053);
#2249=CIRCLE('',#7134,3.68751484013274);
#2250=CIRCLE('',#7135,3.68751484013275);
#2251=CIRCLE('',#7136,0.269999999999999);
#2252=CIRCLE('',#7137,12.3750000000023);
#2253=CIRCLE('',#7138,3.68751484013276);
#2254=CIRCLE('',#7139,3.68751484013273);
#2255=CIRCLE('',#7140,0.269999999999998);
#2256=CIRCLE('',#7141,12.3749999999973);
#2257=CIRCLE('',#7142,3.68751484013274);
#2258=CIRCLE('',#7143,3.68751484013276);
#2259=CIRCLE('',#7144,0.269999999999999);
#2260=CIRCLE('',#7145,12.3749999999999);
#2261=CIRCLE('',#7146,3.68751484013273);
#2262=CIRCLE('',#7147,3.68751484013276);
#2263=CIRCLE('',#7148,0.269999999999998);
#2264=CIRCLE('',#7149,12.3749999999996);
#2265=CIRCLE('',#7150,3.68751484013273);
#2266=CIRCLE('',#7151,3.68751484013272);
#2267=CIRCLE('',#7152,0.270000000000001);
#2268=CIRCLE('',#7153,12.3750000000059);
#2269=CIRCLE('',#7154,3.68751484013275);
#2270=CIRCLE('',#7155,0.269999999999999);
#2271=CIRCLE('',#7156,12.3750000000028);
#2272=CIRCLE('',#7157,14.3999999999998);
#2273=CIRCLE('',#7158,3.68751484013274);
#2274=CIRCLE('',#7159,0.269999999999999);
#2275=CIRCLE('',#7160,12.3749999999925);
#2276=CIRCLE('',#7161,0.269999999999996);
#2277=CIRCLE('',#7162,3.68751484013274);
#2278=CIRCLE('',#7163,3.68751484013274);
#2279=CIRCLE('',#7164,0.269999999999998);
#2280=CIRCLE('',#7165,12.3750000000028);
#2281=CIRCLE('',#7166,0.27);
#2282=CIRCLE('',#7167,3.68751484013274);
#2283=CIRCLE('',#7168,3.68751484013275);
#2284=CIRCLE('',#7169,0.269999999999999);
#2285=CIRCLE('',#7170,12.3750000000005);
#2286=CIRCLE('',#7171,0.269999999999999);
#2287=CIRCLE('',#7172,3.68751484013275);
#2288=CIRCLE('',#7173,3.68751484013275);
#2289=CIRCLE('',#7174,0.269999999999999);
#2290=CIRCLE('',#7175,12.3749999999995);
#2291=CIRCLE('',#7176,0.270000000000001);
#2292=CIRCLE('',#7177,3.68751484013273);
#2293=CIRCLE('',#7179,3.68751484013276);
#2294=CIRCLE('',#7180,3.68751484013275);
#2295=CIRCLE('',#7181,0.270000000000002);
#2296=CIRCLE('',#7182,12.3749999999995);
#2297=CIRCLE('',#7183,0.269999999999999);
#2298=CIRCLE('',#7184,3.68751484013274);
#2299=CIRCLE('',#7185,3.68751484013275);
#2300=CIRCLE('',#7186,0.269999999999999);
#2301=CIRCLE('',#7187,12.3750000000005);
#2302=CIRCLE('',#7188,0.269999999999999);
#2303=CIRCLE('',#7189,3.68751484013275);
#2304=CIRCLE('',#7190,3.68751484013275);
#2305=CIRCLE('',#7191,0.27);
#2306=CIRCLE('',#7192,12.3750000000028);
#2307=CIRCLE('',#7193,0.269999999999998);
#2308=CIRCLE('',#7194,3.68751484013275);
#2309=CIRCLE('',#7195,3.68751484013274);
#2310=CIRCLE('',#7196,0.269999999999996);
#2311=CIRCLE('',#7197,12.3749999999925);
#2312=CIRCLE('',#7198,0.269999999999999);
#2313=CIRCLE('',#7199,3.68751484013274);
#2314=CIRCLE('',#7200,14.3999999999958);
#2315=CIRCLE('',#7201,12.3750000000028);
#2316=CIRCLE('',#7202,0.269999999999999);
#2317=CIRCLE('',#7203,3.68751484013275);
#2318=CIRCLE('',#7204,12.3750000000059);
#2319=CIRCLE('',#7205,0.270000000000001);
#2320=CIRCLE('',#7206,3.68751484013271);
#2321=CIRCLE('',#7207,3.68751484013274);
#2322=CIRCLE('',#7208,12.3749999999996);
#2323=CIRCLE('',#7209,0.269999999999997);
#2324=CIRCLE('',#7210,3.68751484013275);
#2325=CIRCLE('',#7211,3.68751484013273);
#2326=CIRCLE('',#7212,12.3749999999999);
#2327=CIRCLE('',#7213,0.269999999999999);
#2328=CIRCLE('',#7214,3.68751484013275);
#2329=CIRCLE('',#7215,3.68751484013273);
#2330=CIRCLE('',#7216,12.3749999999973);
#2331=CIRCLE('',#7217,0.269999999999998);
#2332=CIRCLE('',#7218,3.68751484013274);
#2333=CIRCLE('',#7219,3.68751484013274);
#2334=CIRCLE('',#7220,12.3750000000023);
#2335=CIRCLE('',#7221,0.269999999999999);
#2336=CIRCLE('',#7222,3.68751484013275);
#2337=CIRCLE('',#7223,3.68751484013276);
#2338=CIRCLE('',#7224,12.3750000000053);
#2339=CIRCLE('',#7225,0.270000000000001);
#2340=CIRCLE('',#7226,3.68751484013274);
#2341=CIRCLE('',#7227,3.68751484013275);
#2342=CIRCLE('',#7228,0.270000000000001);
#2343=CIRCLE('',#7229,12.3750000000014);
#2344=CIRCLE('',#7230,3.68751484013273);
#2345=CIRCLE('',#7231,3.68751484013274);
#2346=CIRCLE('',#7232,0.270000000000001);
#2347=CIRCLE('',#7233,12.3749999999985);
#2348=CIRCLE('',#7234,3.68751484013275);
#2349=CIRCLE('',#7235,3.68751484013276);
#2350=CIRCLE('',#7236,0.269999999999999);
#2351=CIRCLE('',#7237,12.3750000000006);
#2352=CIRCLE('',#7238,3.68751484013272);
#2353=CIRCLE('',#7239,3.68751484013277);
#2354=CIRCLE('',#7240,0.269999999999999);
#2355=CIRCLE('',#7241,12.375);
#2356=CIRCLE('',#7242,3.68751484013274);
#2357=CIRCLE('',#7243,3.68751484013274);
#2358=CIRCLE('',#7244,0.269999999999999);
#2359=CIRCLE('',#7245,12.3750000000013);
#2360=CIRCLE('',#7246,3.68751484013273);
#2361=CIRCLE('',#7247,3.68751484013275);
#2362=CIRCLE('',#7248,0.269999999999999);
#2363=CIRCLE('',#7249,12.3750000000026);
#2364=CIRCLE('',#7250,3.68751484013273);
#2365=CIRCLE('',#7251,0.270000000000001);
#2366=CIRCLE('',#7252,12.3749999999951);
#2367=CIRCLE('',#7253,3.68751484013274);
#2368=CIRCLE('',#7254,0.270000000000002);
#2369=CIRCLE('',#7255,12.3749999999924);
#2370=CIRCLE('',#7256,0.270000000000002);
#2371=CIRCLE('',#7257,3.68751484013273);
#2372=CIRCLE('',#7258,3.68751484013274);
#2373=CIRCLE('',#7259,0.27);
#2374=CIRCLE('',#7260,12.374999999999);
#2375=CIRCLE('',#7261,0.27);
#2376=CIRCLE('',#7262,3.68751484013275);
#2377=CIRCLE('',#7263,3.68751484013276);
#2378=CIRCLE('',#7264,0.270000000000002);
#2379=CIRCLE('',#7265,12.3749999999991);
#2380=CIRCLE('',#7266,0.269999999999999);
#2381=CIRCLE('',#7267,3.68751484013275);
#2382=CIRCLE('',#7268,3.68751484013272);
#2383=CIRCLE('',#7269,0.270000000000001);
#2384=CIRCLE('',#7270,12.3750000000007);
#2385=CIRCLE('',#7271,0.270000000000003);
#2386=CIRCLE('',#7272,3.68751484013274);
#2387=CIRCLE('',#7273,3.68751484013273);
#2388=CIRCLE('',#7274,0.269999999999999);
#2389=CIRCLE('',#7275,12.3749999999972);
#2390=CIRCLE('',#7276,0.270000000000003);
#2391=CIRCLE('',#7277,3.68751484013275);
#2392=CIRCLE('',#7278,3.68751484013274);
#2393=CIRCLE('',#7279,0.270000000000001);
#2394=CIRCLE('',#7280,12.3749999999983);
#2395=CIRCLE('',#7281,0.269999999999999);
#2396=CIRCLE('',#7282,3.68751484013274);
#2397=CIRCLE('',#7283,3.68751484013275);
#2398=CIRCLE('',#7284,0.269999999999998);
#2399=CIRCLE('',#7285,12.3750000000045);
#2400=CIRCLE('',#7286,0.270000000000001);
#2401=CIRCLE('',#7287,3.68751484013272);
#2402=CIRCLE('',#7288,3.68751484013277);
#2403=CIRCLE('',#7289,0.269999999999999);
#2404=CIRCLE('',#7290,12.3749999999976);
#2405=CIRCLE('',#7291,0.269999999999998);
#2406=CIRCLE('',#7292,3.68751484013272);
#2407=CIRCLE('',#7293,3.68751484013274);
#2408=CIRCLE('',#7294,0.270000000000001);
#2409=CIRCLE('',#7295,12.3750000000051);
#2410=CIRCLE('',#7296,0.270000000000003);
#2411=CIRCLE('',#7297,3.68751484013273);
#2412=CIRCLE('',#7298,3.68751484013275);
#2413=CIRCLE('',#7299,0.270000000000001);
#2414=CIRCLE('',#7300,12.3750000000098);
#2415=CIRCLE('',#7301,0.270000000000001);
#2416=CIRCLE('',#7302,3.68751484013276);
#2417=CIRCLE('',#7303,3.68751484013275);
#2418=CIRCLE('',#7304,0.269999999999998);
#2419=CIRCLE('',#7305,12.3750000000014);
#2420=CIRCLE('',#7306,0.269999999999999);
#2421=CIRCLE('',#7307,3.68751484013272);
#2422=CIRCLE('',#7308,3.68751484013274);
#2423=CIRCLE('',#7309,0.270000000000001);
#2424=CIRCLE('',#7310,12.3749999999972);
#2425=CIRCLE('',#7311,0.269999999999998);
#2426=CIRCLE('',#7450,1.5);
#2427=CIRCLE('',#7451,1.5);
#2428=CIRCLE('',#7453,5.);
#2429=CIRCLE('',#7454,5.);
#2430=CIRCLE('',#7455,5.);
#2431=CIRCLE('',#7456,5.);
#2432=CIRCLE('',#7458,1.5);
#2433=CIRCLE('',#7459,1.5);
#2434=CIRCLE('',#7461,5.);
#2435=CIRCLE('',#7462,5.);
#2436=CIRCLE('',#7465,5.);
#2437=CIRCLE('',#7466,5.);
#2438=CIRCLE('',#7488,1.25);
#2439=CIRCLE('',#7489,1.25);
#2440=CIRCLE('',#7490,1.25);
#2441=CIRCLE('',#7491,1.25);
#2442=CIRCLE('',#7492,1.25);
#2443=CIRCLE('',#7493,1.25);
#2444=CIRCLE('',#7495,1.5);
#2445=CIRCLE('',#7496,1.5);
#2446=CIRCLE('',#7498,1.5);
#2447=CIRCLE('',#7500,1.5);
#2448=CIRCLE('',#7503,2.5);
#2449=CIRCLE('',#7504,2.5);
#2450=CIRCLE('',#7506,2.5);
#2451=CIRCLE('',#7509,2.5);
#2452=CIRCLE('',#7513,1.5);
#2453=CIRCLE('',#7515,1.5);
#2454=CIRCLE('',#7523,3.5);
#2455=CIRCLE('',#7524,3.5);
#2456=CIRCLE('',#7526,3.5);
#2457=CIRCLE('',#7527,3.5);
#2458=CIRCLE('',#7529,1.5);
#2459=CIRCLE('',#7530,1.5);
#2460=CIRCLE('',#7532,1.5);
#2461=CIRCLE('',#7533,1.5);
#2462=CIRCLE('',#7535,3.5);
#2463=CIRCLE('',#7536,3.5);
#2464=CIRCLE('',#7538,3.5);
#2465=CIRCLE('',#7539,3.5);
#2466=CIRCLE('',#7543,3.5);
#2467=CIRCLE('',#7545,3.5);
#2468=CIRCLE('',#7548,3.5);
#2469=CIRCLE('',#7552,3.5);
#2470=CIRCLE('',#7558,1.25);
#2471=CIRCLE('',#7559,1.25);
#2472=CIRCLE('',#7560,1.25);
#2473=CIRCLE('',#7561,1.25);
#2474=CIRCLE('',#7562,1.25);
#2475=CIRCLE('',#7563,1.25);
#2476=CIRCLE('',#7565,1.5);
#2477=CIRCLE('',#7566,1.5);
#2478=CIRCLE('',#7568,1.5);
#2479=CIRCLE('',#7570,1.5);
#2480=CIRCLE('',#7573,1.5);
#2481=CIRCLE('',#7575,1.5);
#2482=CIRCLE('',#7582,2.5);
#2483=CIRCLE('',#7583,2.5);
#2484=CIRCLE('',#7585,2.5);
#2485=CIRCLE('',#7588,2.5);
#2486=CIRCLE('',#7593,2.5);
#2487=CIRCLE('',#7594,2.5);
#2488=CIRCLE('',#7595,0.1);
#2489=CIRCLE('',#7596,2.4);
#2490=CIRCLE('',#7598,1.25);
#2491=CIRCLE('',#7599,1.25);
#2492=CIRCLE('',#7601,2.5);
#2493=CIRCLE('',#7603,1.5);
#2494=CIRCLE('',#7604,1.5);
#2495=CIRCLE('',#7605,1.5);
#2496=CIRCLE('',#7606,1.5);
#2497=CIRCLE('',#7607,1.5);
#2498=CIRCLE('',#7608,1.5);
#2499=CIRCLE('',#7610,1.25);
#2500=CIRCLE('',#7613,1.25);
#2501=VERTEX_POINT('',#9911);
#2502=VERTEX_POINT('',#9913);
#2503=VERTEX_POINT('',#9917);
#2504=VERTEX_POINT('',#9919);
#2505=VERTEX_POINT('',#9923);
#2506=VERTEX_POINT('',#9925);
#2507=VERTEX_POINT('',#9929);
#2508=VERTEX_POINT('',#9931);
#2509=VERTEX_POINT('',#9935);
#2510=VERTEX_POINT('',#9936);
#2511=VERTEX_POINT('',#9938);
#2512=VERTEX_POINT('',#9940);
#2513=VERTEX_POINT('',#9944);
#2514=VERTEX_POINT('',#9946);
#2515=VERTEX_POINT('',#9950);
#2516=VERTEX_POINT('',#9952);
#2517=VERTEX_POINT('',#9956);
#2518=VERTEX_POINT('',#9958);
#2519=VERTEX_POINT('',#9962);
#2520=VERTEX_POINT('',#9963);
#2521=VERTEX_POINT('',#9965);
#2522=VERTEX_POINT('',#9967);
#2523=VERTEX_POINT('',#9971);
#2524=VERTEX_POINT('',#9972);
#2525=VERTEX_POINT('',#9974);
#2526=VERTEX_POINT('',#9976);
#2527=VERTEX_POINT('',#9980);
#2528=VERTEX_POINT('',#9982);
#2529=VERTEX_POINT('',#9986);
#2530=VERTEX_POINT('',#9988);
#2531=VERTEX_POINT('',#9992);
#2532=VERTEX_POINT('',#9993);
#2533=VERTEX_POINT('',#9995);
#2534=VERTEX_POINT('',#9997);
#2535=VERTEX_POINT('',#10001);
#2536=VERTEX_POINT('',#10003);
#2537=VERTEX_POINT('',#10007);
#2538=VERTEX_POINT('',#10009);
#2539=VERTEX_POINT('',#10013);
#2540=VERTEX_POINT('',#10015);
#2541=VERTEX_POINT('',#10034);
#2542=VERTEX_POINT('',#10036);
#2543=VERTEX_POINT('',#10040);
#2544=VERTEX_POINT('',#10041);
#2545=VERTEX_POINT('',#10043);
#2546=VERTEX_POINT('',#10045);
#2547=VERTEX_POINT('',#10049);
#2548=VERTEX_POINT('',#10050);
#2549=VERTEX_POINT('',#10052);
#2550=VERTEX_POINT('',#10054);
#2551=VERTEX_POINT('',#10058);
#2552=VERTEX_POINT('',#10060);
#2553=VERTEX_POINT('',#10064);
#2554=VERTEX_POINT('',#10066);
#2555=VERTEX_POINT('',#10070);
#2556=VERTEX_POINT('',#10071);
#2557=VERTEX_POINT('',#10073);
#2558=VERTEX_POINT('',#10075);
#2559=VERTEX_POINT('',#10077);
#2560=VERTEX_POINT('',#10079);
#2561=VERTEX_POINT('',#10083);
#2562=VERTEX_POINT('',#10084);
#2563=VERTEX_POINT('',#10087);
#2564=VERTEX_POINT('',#10089);
#2565=VERTEX_POINT('',#10093);
#2566=VERTEX_POINT('',#10094);
#2567=VERTEX_POINT('',#10099);
#2568=VERTEX_POINT('',#10101);
#2569=VERTEX_POINT('',#10104);
#2570=VERTEX_POINT('',#10106);
#2571=VERTEX_POINT('',#10115);
#2572=VERTEX_POINT('',#10117);
#2573=VERTEX_POINT('',#10126);
#2574=VERTEX_POINT('',#10130);
#2575=VERTEX_POINT('',#10137);
#2576=VERTEX_POINT('',#10139);
#2577=VERTEX_POINT('',#10143);
#2578=VERTEX_POINT('',#10145);
#2579=VERTEX_POINT('',#10149);
#2580=VERTEX_POINT('',#10153);
#2581=VERTEX_POINT('',#10162);
#2582=VERTEX_POINT('',#10164);
#2583=VERTEX_POINT('',#10168);
#2584=VERTEX_POINT('',#10169);
#2585=VERTEX_POINT('',#10171);
#2586=VERTEX_POINT('',#10173);
#2587=VERTEX_POINT('',#10177);
#2588=VERTEX_POINT('',#10179);
#2589=VERTEX_POINT('',#10183);
#2590=VERTEX_POINT('',#10184);
#2591=VERTEX_POINT('',#10186);
#2592=VERTEX_POINT('',#10188);
#2593=VERTEX_POINT('',#10192);
#2594=VERTEX_POINT('',#10193);
#2595=VERTEX_POINT('',#10195);
#2596=VERTEX_POINT('',#10197);
#2597=VERTEX_POINT('',#10201);
#2598=VERTEX_POINT('',#10203);
#2599=VERTEX_POINT('',#10207);
#2600=VERTEX_POINT('',#10209);
#2601=VERTEX_POINT('',#10213);
#2602=VERTEX_POINT('',#10215);
#2603=VERTEX_POINT('',#10219);
#2604=VERTEX_POINT('',#10220);
#2605=VERTEX_POINT('',#10222);
#2606=VERTEX_POINT('',#10224);
#2607=VERTEX_POINT('',#10226);
#2608=VERTEX_POINT('',#10228);
#2609=VERTEX_POINT('',#10230);
#2610=VERTEX_POINT('',#10232);
#2611=VERTEX_POINT('',#10235);
#2612=VERTEX_POINT('',#10236);
#2613=VERTEX_POINT('',#10241);
#2614=VERTEX_POINT('',#10243);
#2615=VERTEX_POINT('',#10246);
#2616=VERTEX_POINT('',#10248);
#2617=VERTEX_POINT('',#10259);
#2618=VERTEX_POINT('',#10261);
#2619=VERTEX_POINT('',#10270);
#2620=VERTEX_POINT('',#10274);
#2621=VERTEX_POINT('',#10281);
#2622=VERTEX_POINT('',#10283);
#2623=VERTEX_POINT('',#10287);
#2624=VERTEX_POINT('',#10291);
#2625=VERTEX_POINT('',#10300);
#2626=VERTEX_POINT('',#10301);
#2627=VERTEX_POINT('',#10303);
#2628=VERTEX_POINT('',#10305);
#2629=VERTEX_POINT('',#10309);
#2630=VERTEX_POINT('',#10310);
#2631=VERTEX_POINT('',#10312);
#2632=VERTEX_POINT('',#10314);
#2633=VERTEX_POINT('',#10318);
#2634=VERTEX_POINT('',#10320);
#2635=VERTEX_POINT('',#10324);
#2636=VERTEX_POINT('',#10325);
#2637=VERTEX_POINT('',#10327);
#2638=VERTEX_POINT('',#10329);
#2639=VERTEX_POINT('',#10333);
#2640=VERTEX_POINT('',#10335);
#2641=VERTEX_POINT('',#10339);
#2642=VERTEX_POINT('',#10340);
#2643=VERTEX_POINT('',#10342);
#2644=VERTEX_POINT('',#10344);
#2645=VERTEX_POINT('',#10348);
#2646=VERTEX_POINT('',#10350);
#2647=VERTEX_POINT('',#10354);
#2648=VERTEX_POINT('',#10355);
#2649=VERTEX_POINT('',#10357);
#2650=VERTEX_POINT('',#10359);
#2651=VERTEX_POINT('',#10363);
#2652=VERTEX_POINT('',#10365);
#2653=VERTEX_POINT('',#10369);
#2654=VERTEX_POINT('',#10370);
#2655=VERTEX_POINT('',#10372);
#2656=VERTEX_POINT('',#10374);
#2657=VERTEX_POINT('',#10378);
#2658=VERTEX_POINT('',#10379);
#2659=VERTEX_POINT('',#10381);
#2660=VERTEX_POINT('',#10383);
#2661=VERTEX_POINT('',#10387);
#2662=VERTEX_POINT('',#10388);
#2663=VERTEX_POINT('',#10390);
#2664=VERTEX_POINT('',#10392);
#2665=VERTEX_POINT('',#10396);
#2666=VERTEX_POINT('',#10397);
#2667=VERTEX_POINT('',#10399);
#2668=VERTEX_POINT('',#10401);
#2669=VERTEX_POINT('',#10405);
#2670=VERTEX_POINT('',#10406);
#2671=VERTEX_POINT('',#10408);
#2672=VERTEX_POINT('',#10410);
#2673=VERTEX_POINT('',#10414);
#2674=VERTEX_POINT('',#10415);
#2675=VERTEX_POINT('',#10417);
#2676=VERTEX_POINT('',#10419);
#2677=VERTEX_POINT('',#10423);
#2678=VERTEX_POINT('',#10424);
#2679=VERTEX_POINT('',#10426);
#2680=VERTEX_POINT('',#10428);
#2681=VERTEX_POINT('',#10432);
#2682=VERTEX_POINT('',#10433);
#2683=VERTEX_POINT('',#10435);
#2684=VERTEX_POINT('',#10437);
#2685=VERTEX_POINT('',#10441);
#2686=VERTEX_POINT('',#10442);
#2687=VERTEX_POINT('',#10444);
#2688=VERTEX_POINT('',#10446);
#2689=VERTEX_POINT('',#10450);
#2690=VERTEX_POINT('',#10451);
#2691=VERTEX_POINT('',#10453);
#2692=VERTEX_POINT('',#10455);
#2693=VERTEX_POINT('',#10459);
#2694=VERTEX_POINT('',#10460);
#2695=VERTEX_POINT('',#10462);
#2696=VERTEX_POINT('',#10464);
#2697=VERTEX_POINT('',#10468);
#2698=VERTEX_POINT('',#10469);
#2699=VERTEX_POINT('',#10471);
#2700=VERTEX_POINT('',#10473);
#2701=VERTEX_POINT('',#10477);
#2702=VERTEX_POINT('',#10478);
#2703=VERTEX_POINT('',#10480);
#2704=VERTEX_POINT('',#10482);
#2705=VERTEX_POINT('',#10486);
#2706=VERTEX_POINT('',#10487);
#2707=VERTEX_POINT('',#10489);
#2708=VERTEX_POINT('',#10491);
#2709=VERTEX_POINT('',#10495);
#2710=VERTEX_POINT('',#10496);
#2711=VERTEX_POINT('',#10498);
#2712=VERTEX_POINT('',#10500);
#2713=VERTEX_POINT('',#10504);
#2714=VERTEX_POINT('',#10505);
#2715=VERTEX_POINT('',#10507);
#2716=VERTEX_POINT('',#10509);
#2717=VERTEX_POINT('',#10513);
#2718=VERTEX_POINT('',#10514);
#2719=VERTEX_POINT('',#10516);
#2720=VERTEX_POINT('',#10518);
#2721=VERTEX_POINT('',#10522);
#2722=VERTEX_POINT('',#10523);
#2723=VERTEX_POINT('',#10525);
#2724=VERTEX_POINT('',#10527);
#2725=VERTEX_POINT('',#10531);
#2726=VERTEX_POINT('',#10532);
#2727=VERTEX_POINT('',#10534);
#2728=VERTEX_POINT('',#10536);
#2729=VERTEX_POINT('',#10540);
#2730=VERTEX_POINT('',#10541);
#2731=VERTEX_POINT('',#10543);
#2732=VERTEX_POINT('',#10545);
#2733=VERTEX_POINT('',#10549);
#2734=VERTEX_POINT('',#10550);
#2735=VERTEX_POINT('',#10552);
#2736=VERTEX_POINT('',#10554);
#2737=VERTEX_POINT('',#10558);
#2738=VERTEX_POINT('',#10559);
#2739=VERTEX_POINT('',#10561);
#2740=VERTEX_POINT('',#10563);
#2741=VERTEX_POINT('',#10567);
#2742=VERTEX_POINT('',#10568);
#2743=VERTEX_POINT('',#10570);
#2744=VERTEX_POINT('',#10572);
#2745=VERTEX_POINT('',#10576);
#2746=VERTEX_POINT('',#10577);
#2747=VERTEX_POINT('',#10579);
#2748=VERTEX_POINT('',#10581);
#2749=VERTEX_POINT('',#10585);
#2750=VERTEX_POINT('',#10587);
#2751=VERTEX_POINT('',#10591);
#2752=VERTEX_POINT('',#10593);
#2753=VERTEX_POINT('',#10597);
#2754=VERTEX_POINT('',#10599);
#2755=VERTEX_POINT('',#10603);
#2756=VERTEX_POINT('',#10604);
#2757=VERTEX_POINT('',#10606);
#2758=VERTEX_POINT('',#10608);
#2759=VERTEX_POINT('',#10612);
#2760=VERTEX_POINT('',#10613);
#2761=VERTEX_POINT('',#10615);
#2762=VERTEX_POINT('',#10617);
#2763=VERTEX_POINT('',#10621);
#2764=VERTEX_POINT('',#10622);
#2765=VERTEX_POINT('',#10624);
#2766=VERTEX_POINT('',#10626);
#2767=VERTEX_POINT('',#10630);
#2768=VERTEX_POINT('',#10631);
#2769=VERTEX_POINT('',#10633);
#2770=VERTEX_POINT('',#10635);
#2771=VERTEX_POINT('',#10639);
#2772=VERTEX_POINT('',#10640);
#2773=VERTEX_POINT('',#10642);
#2774=VERTEX_POINT('',#10644);
#2775=VERTEX_POINT('',#10648);
#2776=VERTEX_POINT('',#10649);
#2777=VERTEX_POINT('',#10651);
#2778=VERTEX_POINT('',#10653);
#2779=VERTEX_POINT('',#10657);
#2780=VERTEX_POINT('',#10658);
#2781=VERTEX_POINT('',#10660);
#2782=VERTEX_POINT('',#10662);
#2783=VERTEX_POINT('',#10666);
#2784=VERTEX_POINT('',#10667);
#2785=VERTEX_POINT('',#10669);
#2786=VERTEX_POINT('',#10671);
#2787=VERTEX_POINT('',#10675);
#2788=VERTEX_POINT('',#10676);
#2789=VERTEX_POINT('',#10678);
#2790=VERTEX_POINT('',#10680);
#2791=VERTEX_POINT('',#10684);
#2792=VERTEX_POINT('',#10685);
#2793=VERTEX_POINT('',#10687);
#2794=VERTEX_POINT('',#10689);
#2795=VERTEX_POINT('',#10693);
#2796=VERTEX_POINT('',#10694);
#2797=VERTEX_POINT('',#10696);
#2798=VERTEX_POINT('',#10698);
#2799=VERTEX_POINT('',#10702);
#2800=VERTEX_POINT('',#10703);
#2801=VERTEX_POINT('',#10705);
#2802=VERTEX_POINT('',#10707);
#2803=VERTEX_POINT('',#10711);
#2804=VERTEX_POINT('',#10713);
#2805=VERTEX_POINT('',#10715);
#2806=VERTEX_POINT('',#10717);
#2807=VERTEX_POINT('',#10720);
#2808=VERTEX_POINT('',#10722);
#2809=VERTEX_POINT('',#10724);
#2810=VERTEX_POINT('',#10726);
#2811=VERTEX_POINT('',#10729);
#2812=VERTEX_POINT('',#10731);
#2813=VERTEX_POINT('',#10733);
#2814=VERTEX_POINT('',#10735);
#2815=VERTEX_POINT('',#10738);
#2816=VERTEX_POINT('',#10740);
#2817=VERTEX_POINT('',#10742);
#2818=VERTEX_POINT('',#10744);
#2819=VERTEX_POINT('',#10747);
#2820=VERTEX_POINT('',#10749);
#2821=VERTEX_POINT('',#10751);
#2822=VERTEX_POINT('',#10753);
#2823=VERTEX_POINT('',#10756);
#2824=VERTEX_POINT('',#10758);
#2825=VERTEX_POINT('',#10760);
#2826=VERTEX_POINT('',#10762);
#2827=VERTEX_POINT('',#10765);
#2828=VERTEX_POINT('',#10767);
#2829=VERTEX_POINT('',#10769);
#2830=VERTEX_POINT('',#10771);
#2831=VERTEX_POINT('',#10774);
#2832=VERTEX_POINT('',#10776);
#2833=VERTEX_POINT('',#10778);
#2834=VERTEX_POINT('',#10780);
#2835=VERTEX_POINT('',#10783);
#2836=VERTEX_POINT('',#10785);
#2837=VERTEX_POINT('',#10787);
#2838=VERTEX_POINT('',#10789);
#2839=VERTEX_POINT('',#10792);
#2840=VERTEX_POINT('',#10794);
#2841=VERTEX_POINT('',#10796);
#2842=VERTEX_POINT('',#10798);
#2843=VERTEX_POINT('',#10801);
#2844=VERTEX_POINT('',#10803);
#2845=VERTEX_POINT('',#10805);
#2846=VERTEX_POINT('',#10807);
#2847=VERTEX_POINT('',#10810);
#2848=VERTEX_POINT('',#10812);
#2849=VERTEX_POINT('',#10814);
#2850=VERTEX_POINT('',#10816);
#2851=VERTEX_POINT('',#10819);
#2852=VERTEX_POINT('',#10821);
#2853=VERTEX_POINT('',#10824);
#2854=VERTEX_POINT('',#10826);
#2855=VERTEX_POINT('',#10830);
#2856=VERTEX_POINT('',#10832);
#2857=VERTEX_POINT('',#10836);
#2858=VERTEX_POINT('',#10838);
#2859=VERTEX_POINT('',#10842);
#2860=VERTEX_POINT('',#10844);
#2861=VERTEX_POINT('',#10848);
#2862=VERTEX_POINT('',#10850);
#2863=VERTEX_POINT('',#10854);
#2864=VERTEX_POINT('',#10856);
#2865=VERTEX_POINT('',#10859);
#2866=VERTEX_POINT('',#10861);
#2867=VERTEX_POINT('',#10865);
#2868=VERTEX_POINT('',#10867);
#2869=VERTEX_POINT('',#10871);
#2870=VERTEX_POINT('',#10873);
#2871=VERTEX_POINT('',#10877);
#2872=VERTEX_POINT('',#10879);
#2873=VERTEX_POINT('',#10883);
#2874=VERTEX_POINT('',#10885);
#2875=VERTEX_POINT('',#10889);
#2876=VERTEX_POINT('',#10891);
#2877=VERTEX_POINT('',#10894);
#2878=VERTEX_POINT('',#10896);
#2879=VERTEX_POINT('',#10899);
#2880=VERTEX_POINT('',#10901);
#2881=VERTEX_POINT('',#10903);
#2882=VERTEX_POINT('',#10905);
#2883=VERTEX_POINT('',#10907);
#2884=VERTEX_POINT('',#10910);
#2885=VERTEX_POINT('',#10912);
#2886=VERTEX_POINT('',#10914);
#2887=VERTEX_POINT('',#10916);
#2888=VERTEX_POINT('',#10919);
#2889=VERTEX_POINT('',#10921);
#2890=VERTEX_POINT('',#10923);
#2891=VERTEX_POINT('',#10925);
#2892=VERTEX_POINT('',#10928);
#2893=VERTEX_POINT('',#10930);
#2894=VERTEX_POINT('',#10932);
#2895=VERTEX_POINT('',#10934);
#2896=VERTEX_POINT('',#10937);
#2897=VERTEX_POINT('',#10939);
#2898=VERTEX_POINT('',#10943);
#2899=VERTEX_POINT('',#10945);
#2900=VERTEX_POINT('',#10947);
#2901=VERTEX_POINT('',#10949);
#2902=VERTEX_POINT('',#10951);
#2903=VERTEX_POINT('',#10954);
#2904=VERTEX_POINT('',#10956);
#2905=VERTEX_POINT('',#10958);
#2906=VERTEX_POINT('',#10960);
#2907=VERTEX_POINT('',#10963);
#2908=VERTEX_POINT('',#10965);
#2909=VERTEX_POINT('',#10967);
#2910=VERTEX_POINT('',#10969);
#2911=VERTEX_POINT('',#10972);
#2912=VERTEX_POINT('',#10974);
#2913=VERTEX_POINT('',#10976);
#2914=VERTEX_POINT('',#10978);
#2915=VERTEX_POINT('',#10980);
#2916=VERTEX_POINT('',#10983);
#2917=VERTEX_POINT('',#10985);
#2918=VERTEX_POINT('',#10988);
#2919=VERTEX_POINT('',#10990);
#2920=VERTEX_POINT('',#10994);
#2921=VERTEX_POINT('',#10996);
#2922=VERTEX_POINT('',#11000);
#2923=VERTEX_POINT('',#11002);
#2924=VERTEX_POINT('',#11006);
#2925=VERTEX_POINT('',#11008);
#2926=VERTEX_POINT('',#11012);
#2927=VERTEX_POINT('',#11014);
#2928=VERTEX_POINT('',#11018);
#2929=VERTEX_POINT('',#11020);
#2930=VERTEX_POINT('',#11023);
#2931=VERTEX_POINT('',#11025);
#2932=VERTEX_POINT('',#11029);
#2933=VERTEX_POINT('',#11031);
#2934=VERTEX_POINT('',#11035);
#2935=VERTEX_POINT('',#11037);
#2936=VERTEX_POINT('',#11041);
#2937=VERTEX_POINT('',#11043);
#2938=VERTEX_POINT('',#11047);
#2939=VERTEX_POINT('',#11049);
#2940=VERTEX_POINT('',#11053);
#2941=VERTEX_POINT('',#11055);
#2942=VERTEX_POINT('',#11058);
#2943=VERTEX_POINT('',#11060);
#2944=VERTEX_POINT('',#11063);
#2945=VERTEX_POINT('',#11065);
#2946=VERTEX_POINT('',#11067);
#2947=VERTEX_POINT('',#11069);
#2948=VERTEX_POINT('',#11072);
#2949=VERTEX_POINT('',#11074);
#2950=VERTEX_POINT('',#11076);
#2951=VERTEX_POINT('',#11078);
#2952=VERTEX_POINT('',#11081);
#2953=VERTEX_POINT('',#11083);
#2954=VERTEX_POINT('',#11085);
#2955=VERTEX_POINT('',#11087);
#2956=VERTEX_POINT('',#11090);
#2957=VERTEX_POINT('',#11092);
#2958=VERTEX_POINT('',#11094);
#2959=VERTEX_POINT('',#11096);
#2960=VERTEX_POINT('',#11099);
#2961=VERTEX_POINT('',#11101);
#2962=VERTEX_POINT('',#11103);
#2963=VERTEX_POINT('',#11105);
#2964=VERTEX_POINT('',#11108);
#2965=VERTEX_POINT('',#11110);
#2966=VERTEX_POINT('',#11112);
#2967=VERTEX_POINT('',#11114);
#2968=VERTEX_POINT('',#11117);
#2969=VERTEX_POINT('',#11119);
#2970=VERTEX_POINT('',#11121);
#2971=VERTEX_POINT('',#11123);
#2972=VERTEX_POINT('',#11126);
#2973=VERTEX_POINT('',#11128);
#2974=VERTEX_POINT('',#11130);
#2975=VERTEX_POINT('',#11132);
#2976=VERTEX_POINT('',#11135);
#2977=VERTEX_POINT('',#11137);
#2978=VERTEX_POINT('',#11139);
#2979=VERTEX_POINT('',#11141);
#2980=VERTEX_POINT('',#11144);
#2981=VERTEX_POINT('',#11146);
#2982=VERTEX_POINT('',#11148);
#2983=VERTEX_POINT('',#11150);
#2984=VERTEX_POINT('',#11153);
#2985=VERTEX_POINT('',#11155);
#2986=VERTEX_POINT('',#11157);
#2987=VERTEX_POINT('',#11159);
#2988=VERTEX_POINT('',#11162);
#2989=VERTEX_POINT('',#11164);
#2990=VERTEX_POINT('',#11166);
#2991=VERTEX_POINT('',#11169);
#2992=VERTEX_POINT('',#11171);
#2993=VERTEX_POINT('',#11407);
#2994=VERTEX_POINT('',#11409);
#2995=VERTEX_POINT('',#11413);
#2996=VERTEX_POINT('',#11414);
#2997=VERTEX_POINT('',#11416);
#2998=VERTEX_POINT('',#11418);
#2999=VERTEX_POINT('',#11420);
#3000=VERTEX_POINT('',#11422);
#3001=VERTEX_POINT('',#11424);
#3002=VERTEX_POINT('',#11426);
#3003=VERTEX_POINT('',#11430);
#3004=VERTEX_POINT('',#11432);
#3005=VERTEX_POINT('',#11436);
#3006=VERTEX_POINT('',#11437);
#3007=VERTEX_POINT('',#11439);
#3008=VERTEX_POINT('',#11441);
#3009=VERTEX_POINT('',#11443);
#3010=VERTEX_POINT('',#11446);
#3011=VERTEX_POINT('',#11448);
#3012=VERTEX_POINT('',#11450);
#3013=VERTEX_POINT('',#11452);
#3014=VERTEX_POINT('',#11456);
#3015=VERTEX_POINT('',#11458);
#3016=VERTEX_POINT('',#11460);
#3017=VERTEX_POINT('',#11462);
#3018=VERTEX_POINT('',#11466);
#3019=VERTEX_POINT('',#11467);
#3020=VERTEX_POINT('',#11469);
#3021=VERTEX_POINT('',#11471);
#3022=VERTEX_POINT('',#11473);
#3023=VERTEX_POINT('',#11475);
#3024=VERTEX_POINT('',#11477);
#3025=VERTEX_POINT('',#11480);
#3026=VERTEX_POINT('',#11482);
#3027=VERTEX_POINT('',#11486);
#3028=VERTEX_POINT('',#11487);
#3029=VERTEX_POINT('',#11490);
#3030=VERTEX_POINT('',#11492);
#3031=VERTEX_POINT('',#11511);
#3032=VERTEX_POINT('',#11513);
#3033=VERTEX_POINT('',#11515);
#3034=VERTEX_POINT('',#11517);
#3035=VERTEX_POINT('',#11521);
#3036=VERTEX_POINT('',#11523);
#3037=VERTEX_POINT('',#11528);
#3038=VERTEX_POINT('',#11531);
#3039=VERTEX_POINT('',#11548);
#3040=VERTEX_POINT('',#11550);
#3041=VERTEX_POINT('',#11552);
#3042=VERTEX_POINT('',#11554);
#3043=VERTEX_POINT('',#11556);
#3044=VERTEX_POINT('',#11558);
#3045=VERTEX_POINT('',#11560);
#3046=VERTEX_POINT('',#11562);
#3047=VERTEX_POINT('',#11564);
#3048=VERTEX_POINT('',#11566);
#3049=VERTEX_POINT('',#11570);
#3050=VERTEX_POINT('',#11572);
#3051=VERTEX_POINT('',#11576);
#3052=VERTEX_POINT('',#11578);
#3053=VERTEX_POINT('',#11582);
#3054=VERTEX_POINT('',#11584);
#3055=VERTEX_POINT('',#11589);
#3056=VERTEX_POINT('',#11590);
#3057=VERTEX_POINT('',#11592);
#3058=VERTEX_POINT('',#11594);
#3059=VERTEX_POINT('',#11598);
#3060=VERTEX_POINT('',#11599);
#3061=VERTEX_POINT('',#11604);
#3062=VERTEX_POINT('',#11608);
#3063=VERTEX_POINT('',#11615);
#3064=VERTEX_POINT('',#11616);
#3065=VERTEX_POINT('',#11621);
#3066=VERTEX_POINT('',#11622);
#3067=VERTEX_POINT('',#11637);
#3068=VERTEX_POINT('',#11638);
#3069=VERTEX_POINT('',#11640);
#3070=VERTEX_POINT('',#11642);
#3071=VERTEX_POINT('',#11646);
#3072=VERTEX_POINT('',#11647);
#3073=VERTEX_POINT('',#11649);
#3074=VERTEX_POINT('',#11651);
#3075=VERTEX_POINT('',#11655);
#3076=VERTEX_POINT('',#11657);
#3077=VERTEX_POINT('',#11661);
#3078=VERTEX_POINT('',#11663);
#3079=VERTEX_POINT('',#11667);
#3080=VERTEX_POINT('',#11668);
#3081=VERTEX_POINT('',#11670);
#3082=VERTEX_POINT('',#11672);
#3083=VERTEX_POINT('',#11676);
#3084=VERTEX_POINT('',#11678);
#3085=VERTEX_POINT('',#11681);
#3086=VERTEX_POINT('',#11682);
#3087=VERTEX_POINT('',#11687);
#3088=VERTEX_POINT('',#11691);
#3089=VERTEX_POINT('',#11697);
#3090=VERTEX_POINT('',#11699);
#3091=VERTEX_POINT('',#11703);
#3092=VERTEX_POINT('',#11707);
#3093=VERTEX_POINT('',#11714);
#3094=VERTEX_POINT('',#11716);
#3095=VERTEX_POINT('',#11726);
#3096=VERTEX_POINT('',#11728);
#3097=VERTEX_POINT('',#11730);
#3098=VERTEX_POINT('',#11732);
#3099=VERTEX_POINT('',#11734);
#3100=VERTEX_POINT('',#11736);
#3101=VERTEX_POINT('',#11738);
#3102=VERTEX_POINT('',#11740);
#3103=VERTEX_POINT('',#11742);
#3104=VERTEX_POINT('',#11744);
#3105=VERTEX_POINT('',#11748);
#3106=VERTEX_POINT('',#11750);
#3107=VERTEX_POINT('',#11754);
#3108=VERTEX_POINT('',#11756);
#3109=VERTEX_POINT('',#11760);
#3110=VERTEX_POINT('',#11762);
#3111=VERTEX_POINT('',#11767);
#3112=VERTEX_POINT('',#11768);
#3113=VERTEX_POINT('',#11773);
#3114=VERTEX_POINT('',#11774);
#3115=VERTEX_POINT('',#11788);
#3116=VERTEX_POINT('',#11789);
#3117=VERTEX_POINT('',#11791);
#3118=VERTEX_POINT('',#11793);
#3119=VERTEX_POINT('',#11797);
#3120=VERTEX_POINT('',#11799);
#3121=VERTEX_POINT('',#11803);
#3122=VERTEX_POINT('',#11807);
#3123=VERTEX_POINT('',#11815);
#3124=VERTEX_POINT('',#11816);
#3125=VERTEX_POINT('',#11819);
#3126=VERTEX_POINT('',#11823);
#3127=VERTEX_POINT('',#11824);
#3128=VERTEX_POINT('',#11826);
#3129=VERTEX_POINT('',#11828);
#3130=VERTEX_POINT('',#11832);
#3131=VERTEX_POINT('',#11836);
#3132=VERTEX_POINT('',#11837);
#3133=VERTEX_POINT('',#11839);
#3134=VERTEX_POINT('',#11841);
#3135=VERTEX_POINT('',#11843);
#3136=VERTEX_POINT('',#11846);
#3137=VERTEX_POINT('',#11848);
#3138=VERTEX_POINT('',#11850);
#3139=VERTEX_POINT('',#11852);
#3140=VERTEX_POINT('',#11854);
#3141=VERTEX_POINT('',#11858);
#3142=VERTEX_POINT('',#11860);
#3143=VERTEX_POINT('',#11867);
#3144=VERTEX_POINT('',#11869);
#3145=EDGE_CURVE('',#2501,#2501,#1996,.T.);
#3146=EDGE_CURVE('',#2501,#2502,#1072,.T.);
#3147=EDGE_CURVE('',#2502,#2502,#1997,.T.);
#3148=EDGE_CURVE('',#2503,#2503,#1998,.T.);
#3149=EDGE_CURVE('',#2503,#2504,#1073,.T.);
#3150=EDGE_CURVE('',#2504,#2504,#1999,.T.);
#3151=EDGE_CURVE('',#2505,#2505,#2000,.T.);
#3152=EDGE_CURVE('',#2505,#2506,#1074,.T.);
#3153=EDGE_CURVE('',#2506,#2506,#2001,.T.);
#3154=EDGE_CURVE('',#2507,#2507,#2002,.T.);
#3155=EDGE_CURVE('',#2507,#2508,#1075,.T.);
#3156=EDGE_CURVE('',#2508,#2508,#2003,.T.);
#3157=EDGE_CURVE('',#2509,#2510,#1076,.T.);
#3158=EDGE_CURVE('',#2511,#2510,#1077,.T.);
#3159=EDGE_CURVE('',#2512,#2511,#1078,.T.);
#3160=EDGE_CURVE('',#2512,#2509,#1079,.T.);
#3161=EDGE_CURVE('',#2510,#2513,#1080,.T.);
#3162=EDGE_CURVE('',#2514,#2513,#1081,.T.);
#3163=EDGE_CURVE('',#2511,#2514,#1082,.T.);
#3164=EDGE_CURVE('',#2515,#2513,#1083,.T.);
#3165=EDGE_CURVE('',#2516,#2515,#1084,.T.);
#3166=EDGE_CURVE('',#2516,#2514,#1085,.T.);
#3167=EDGE_CURVE('',#2515,#2517,#1086,.T.);
#3168=EDGE_CURVE('',#2517,#2518,#1087,.T.);
#3169=EDGE_CURVE('',#2516,#2518,#1088,.T.);
#3170=EDGE_CURVE('',#2519,#2520,#1089,.T.);
#3171=EDGE_CURVE('',#2519,#2521,#1090,.T.);
#3172=EDGE_CURVE('',#2521,#2522,#1091,.T.);
#3173=EDGE_CURVE('',#2522,#2520,#1092,.T.);
#3174=EDGE_CURVE('',#2523,#2524,#2004,.T.);
#3175=EDGE_CURVE('',#2525,#2523,#1093,.T.);
#3176=EDGE_CURVE('',#2525,#2526,#2005,.T.);
#3177=EDGE_CURVE('',#2526,#2524,#1094,.T.);
#3178=EDGE_CURVE('',#2527,#2523,#2006,.T.);
#3179=EDGE_CURVE('',#2528,#2527,#1095,.T.);
#3180=EDGE_CURVE('',#2528,#2525,#2007,.T.);
#3181=EDGE_CURVE('',#2529,#2527,#1096,.T.);
#3182=EDGE_CURVE('',#2530,#2529,#1097,.T.);
#3183=EDGE_CURVE('',#2530,#2528,#1098,.T.);
#3184=EDGE_CURVE('',#2531,#2532,#2008,.T.);
#3185=EDGE_CURVE('',#2533,#2531,#1099,.T.);
#3186=EDGE_CURVE('',#2533,#2534,#2009,.T.);
#3187=EDGE_CURVE('',#2534,#2532,#1100,.T.);
#3188=EDGE_CURVE('',#2535,#2531,#2010,.T.);
#3189=EDGE_CURVE('',#2536,#2535,#1101,.T.);
#3190=EDGE_CURVE('',#2536,#2533,#2011,.T.);
#3191=EDGE_CURVE('',#2535,#2537,#2012,.T.);
#3192=EDGE_CURVE('',#2538,#2537,#1102,.T.);
#3193=EDGE_CURVE('',#2536,#2538,#2013,.T.);
#3194=EDGE_CURVE('',#2539,#2512,#1103,.T.);
#3195=EDGE_CURVE('',#2539,#2540,#1104,.T.);
#3196=EDGE_CURVE('',#2540,#2509,#1105,.T.);
#3197=EDGE_CURVE('',#2529,#2524,#2014,.T.);
#3198=EDGE_CURVE('',#2530,#2526,#2015,.T.);
#3199=EDGE_CURVE('',#2537,#2532,#1106,.T.);
#3200=EDGE_CURVE('',#2538,#2534,#1107,.T.);
#3201=EDGE_CURVE('',#2518,#2519,#2016,.T.);
#3202=EDGE_CURVE('',#2520,#2539,#2017,.T.);
#3203=EDGE_CURVE('',#2521,#2517,#2018,.T.);
#3204=EDGE_CURVE('',#2540,#2522,#2019,.T.);
#3205=EDGE_CURVE('',#2541,#2541,#2020,.T.);
#3206=EDGE_CURVE('',#2541,#2542,#1108,.T.);
#3207=EDGE_CURVE('',#2542,#2542,#2021,.T.);
#3208=EDGE_CURVE('',#2543,#2544,#2022,.T.);
#3209=EDGE_CURVE('',#2544,#2545,#1109,.T.);
#3210=EDGE_CURVE('',#2546,#2545,#2023,.T.);
#3211=EDGE_CURVE('',#2543,#2546,#1110,.T.);
#3212=EDGE_CURVE('',#2547,#2548,#2024,.T.);
#3213=EDGE_CURVE('',#2547,#2549,#1111,.T.);
#3214=EDGE_CURVE('',#2549,#2550,#2025,.T.);
#3215=EDGE_CURVE('',#2548,#2550,#1112,.T.);
#3216=EDGE_CURVE('',#2551,#2551,#2026,.T.);
#3217=EDGE_CURVE('',#2551,#2552,#1113,.T.);
#3218=EDGE_CURVE('',#2552,#2552,#2027,.T.);
#3219=EDGE_CURVE('',#2553,#2553,#2028,.T.);
#3220=EDGE_CURVE('',#2553,#2554,#1114,.T.);
#3221=EDGE_CURVE('',#2554,#2554,#2029,.T.);
#3222=EDGE_CURVE('',#2555,#2556,#2030,.T.);
#3223=EDGE_CURVE('',#2557,#2555,#2031,.T.);
#3224=EDGE_CURVE('',#2557,#2558,#1115,.T.);
#3225=EDGE_CURVE('',#2558,#2559,#2032,.T.);
#3226=EDGE_CURVE('',#2560,#2559,#1116,.T.);
#3227=EDGE_CURVE('',#2556,#2560,#2033,.T.);
#3228=EDGE_CURVE('',#2561,#2562,#2034,.T.);
#3229=EDGE_CURVE('',#2561,#2556,#1117,.T.);
#3230=EDGE_CURVE('',#2560,#2563,#1118,.T.);
#3231=EDGE_CURVE('',#2563,#2564,#2035,.T.);
#3232=EDGE_CURVE('',#2564,#2557,#1119,.T.);
#3233=EDGE_CURVE('',#2562,#2555,#1120,.T.);
#3234=EDGE_CURVE('',#2565,#2566,#2036,.T.);
#3235=EDGE_CURVE('',#2550,#2565,#1121,.T.);
#3236=EDGE_CURVE('',#2566,#2549,#1122,.T.);
#3237=EDGE_CURVE('',#2567,#2558,#1123,.T.);
#3238=EDGE_CURVE('',#2568,#2567,#2037,.T.);
#3239=EDGE_CURVE('',#2559,#2568,#1124,.T.);
#3240=EDGE_CURVE('',#2545,#2569,#1125,.T.);
#3241=EDGE_CURVE('',#2569,#2570,#2038,.T.);
#3242=EDGE_CURVE('',#2570,#2546,#1126,.T.);
#3243=EDGE_CURVE('',#2563,#2568,#1127,.T.);
#3244=EDGE_CURVE('',#2564,#2567,#1128,.T.);
#3245=EDGE_CURVE('',#2571,#2566,#1129,.T.);
#3246=EDGE_CURVE('',#2572,#2571,#2039,.T.);
#3247=EDGE_CURVE('',#2572,#2565,#1130,.T.);
#3248=EDGE_CURVE('',#2548,#2572,#1131,.T.);
#3249=EDGE_CURVE('',#2571,#2547,#1132,.T.);
#3250=EDGE_CURVE('',#2544,#2573,#1133,.T.);
#3251=EDGE_CURVE('',#2573,#2569,#1134,.T.);
#3252=EDGE_CURVE('',#2573,#2574,#2040,.T.);
#3253=EDGE_CURVE('',#2574,#2570,#1135,.T.);
#3254=EDGE_CURVE('',#2574,#2543,#1136,.T.);
#3255=EDGE_CURVE('',#2555,#2575,#1137,.T.);
#3256=EDGE_CURVE('',#2556,#2576,#1138,.T.);
#3257=EDGE_CURVE('',#2575,#2576,#1139,.T.);
#3258=EDGE_CURVE('',#2577,#2561,#1140,.T.);
#3259=EDGE_CURVE('',#2577,#2578,#1141,.T.);
#3260=EDGE_CURVE('',#2578,#2576,#1142,.T.);
#3261=EDGE_CURVE('',#2579,#2562,#1143,.T.);
#3262=EDGE_CURVE('',#2577,#2579,#2041,.T.);
#3263=EDGE_CURVE('',#2580,#2575,#1144,.T.);
#3264=EDGE_CURVE('',#2579,#2580,#1145,.T.);
#3265=EDGE_CURVE('',#2580,#2578,#1146,.T.);
#3266=EDGE_CURVE('',#2581,#2581,#2042,.T.);
#3267=EDGE_CURVE('',#2581,#2582,#1147,.T.);
#3268=EDGE_CURVE('',#2582,#2582,#2043,.T.);
#3269=EDGE_CURVE('',#2583,#2584,#2044,.T.);
#3270=EDGE_CURVE('',#2583,#2585,#1148,.T.);
#3271=EDGE_CURVE('',#2585,#2586,#2045,.T.);
#3272=EDGE_CURVE('',#2584,#2586,#1149,.T.);
#3273=EDGE_CURVE('',#2587,#2587,#2046,.T.);
#3274=EDGE_CURVE('',#2587,#2588,#1150,.T.);
#3275=EDGE_CURVE('',#2588,#2588,#2047,.T.);
#3276=EDGE_CURVE('',#2589,#2590,#2048,.T.);
#3277=EDGE_CURVE('',#2590,#2591,#1151,.T.);
#3278=EDGE_CURVE('',#2592,#2591,#2049,.T.);
#3279=EDGE_CURVE('',#2589,#2592,#1152,.T.);
#3280=EDGE_CURVE('',#2593,#2594,#2050,.T.);
#3281=EDGE_CURVE('',#2593,#2595,#1153,.T.);
#3282=EDGE_CURVE('',#2595,#2596,#2051,.T.);
#3283=EDGE_CURVE('',#2594,#2596,#1154,.T.);
#3284=EDGE_CURVE('',#2597,#2597,#2052,.T.);
#3285=EDGE_CURVE('',#2597,#2598,#1155,.T.);
#3286=EDGE_CURVE('',#2598,#2598,#2053,.T.);
#3287=EDGE_CURVE('',#2599,#2599,#2054,.T.);
#3288=EDGE_CURVE('',#2599,#2600,#1156,.T.);
#3289=EDGE_CURVE('',#2600,#2600,#2055,.T.);
#3290=EDGE_CURVE('',#2584,#2601,#1157,.T.);
#3291=EDGE_CURVE('',#2602,#2601,#1158,.T.);
#3292=EDGE_CURVE('',#2602,#2583,#1159,.T.);
#3293=EDGE_CURVE('',#2603,#2604,#2056,.T.);
#3294=EDGE_CURVE('',#2603,#2605,#1160,.T.);
#3295=EDGE_CURVE('',#2605,#2606,#1161,.T.);
#3296=EDGE_CURVE('',#2606,#2607,#1162,.T.);
#3297=EDGE_CURVE('',#2607,#2608,#2057,.T.);
#3298=EDGE_CURVE('',#2608,#2609,#1163,.T.);
#3299=EDGE_CURVE('',#2609,#2610,#1164,.T.);
#3300=EDGE_CURVE('',#2604,#2610,#1165,.T.);
#3301=EDGE_CURVE('',#2611,#2612,#2058,.T.);
#3302=EDGE_CURVE('',#2596,#2611,#1166,.T.);
#3303=EDGE_CURVE('',#2612,#2595,#1167,.T.);
#3304=EDGE_CURVE('',#2586,#2613,#1168,.T.);
#3305=EDGE_CURVE('',#2614,#2585,#1169,.T.);
#3306=EDGE_CURVE('',#2613,#2614,#2059,.T.);
#3307=EDGE_CURVE('',#2591,#2615,#1170,.T.);
#3308=EDGE_CURVE('',#2615,#2616,#2060,.T.);
#3309=EDGE_CURVE('',#2616,#2592,#1171,.T.);
#3310=EDGE_CURVE('',#2607,#2613,#1172,.T.);
#3311=EDGE_CURVE('',#2606,#2601,#1173,.T.);
#3312=EDGE_CURVE('',#2608,#2614,#1174,.T.);
#3313=EDGE_CURVE('',#2609,#2602,#1175,.T.);
#3314=EDGE_CURVE('',#2617,#2612,#1176,.T.);
#3315=EDGE_CURVE('',#2618,#2617,#2061,.T.);
#3316=EDGE_CURVE('',#2618,#2611,#1177,.T.);
#3317=EDGE_CURVE('',#2594,#2618,#1178,.T.);
#3318=EDGE_CURVE('',#2617,#2593,#1179,.T.);
#3319=EDGE_CURVE('',#2590,#2619,#1180,.T.);
#3320=EDGE_CURVE('',#2619,#2615,#1181,.T.);
#3321=EDGE_CURVE('',#2619,#2620,#2062,.T.);
#3322=EDGE_CURVE('',#2620,#2616,#1182,.T.);
#3323=EDGE_CURVE('',#2620,#2589,#1183,.T.);
#3324=EDGE_CURVE('',#2621,#2603,#1184,.T.);
#3325=EDGE_CURVE('',#2621,#2622,#1185,.T.);
#3326=EDGE_CURVE('',#2622,#2605,#1186,.T.);
#3327=EDGE_CURVE('',#2623,#2604,#1187,.T.);
#3328=EDGE_CURVE('',#2621,#2623,#2063,.T.);
#3329=EDGE_CURVE('',#2624,#2610,#1188,.T.);
#3330=EDGE_CURVE('',#2623,#2624,#1189,.T.);
#3331=EDGE_CURVE('',#2624,#2622,#1190,.T.);
#3332=EDGE_CURVE('',#2625,#2626,#2064,.T.);
#3333=EDGE_CURVE('',#2625,#2627,#1191,.T.);
#3334=EDGE_CURVE('',#2627,#2628,#2065,.T.);
#3335=EDGE_CURVE('',#2626,#2628,#1192,.T.);
#3336=EDGE_CURVE('',#2629,#2630,#2066,.T.);
#3337=EDGE_CURVE('',#2631,#2629,#1193,.T.);
#3338=EDGE_CURVE('',#2632,#2631,#2067,.T.);
#3339=EDGE_CURVE('',#2630,#2632,#1194,.T.);
#3340=EDGE_CURVE('',#2633,#2632,#2068,.T.);
#3341=EDGE_CURVE('',#2634,#2633,#1195,.T.);
#3342=EDGE_CURVE('',#2634,#2630,#2069,.T.);
#3343=EDGE_CURVE('',#2635,#2636,#2070,.T.);
#3344=EDGE_CURVE('',#2637,#2635,#1196,.T.);
#3345=EDGE_CURVE('',#2638,#2637,#2071,.T.);
#3346=EDGE_CURVE('',#2636,#2638,#1197,.T.);
#3347=EDGE_CURVE('',#2639,#2638,#2072,.T.);
#3348=EDGE_CURVE('',#2640,#2639,#1198,.T.);
#3349=EDGE_CURVE('',#2640,#2636,#2073,.T.);
#3350=EDGE_CURVE('',#2641,#2642,#2074,.T.);
#3351=EDGE_CURVE('',#2643,#2641,#1199,.T.);
#3352=EDGE_CURVE('',#2644,#2643,#2075,.T.);
#3353=EDGE_CURVE('',#2642,#2644,#1200,.T.);
#3354=EDGE_CURVE('',#2643,#2645,#2076,.T.);
#3355=EDGE_CURVE('',#2641,#2646,#2077,.T.);
#3356=EDGE_CURVE('',#2645,#2646,#1201,.T.);
#3357=EDGE_CURVE('',#2647,#2648,#2078,.T.);
#3358=EDGE_CURVE('',#2649,#2647,#1202,.T.);
#3359=EDGE_CURVE('',#2650,#2649,#2079,.T.);
#3360=EDGE_CURVE('',#2648,#2650,#1203,.T.);
#3361=EDGE_CURVE('',#2649,#2651,#2080,.T.);
#3362=EDGE_CURVE('',#2647,#2652,#2081,.T.);
#3363=EDGE_CURVE('',#2651,#2652,#1204,.T.);
#3364=EDGE_CURVE('',#2653,#2654,#2082,.T.);
#3365=EDGE_CURVE('',#2655,#2653,#1205,.T.);
#3366=EDGE_CURVE('',#2656,#2655,#2083,.T.);
#3367=EDGE_CURVE('',#2654,#2656,#1206,.T.);
#3368=EDGE_CURVE('',#2657,#2658,#2084,.T.);
#3369=EDGE_CURVE('',#2659,#2657,#1207,.T.);
#3370=EDGE_CURVE('',#2660,#2659,#2085,.T.);
#3371=EDGE_CURVE('',#2658,#2660,#1208,.T.);
#3372=EDGE_CURVE('',#2661,#2662,#2086,.T.);
#3373=EDGE_CURVE('',#2663,#2661,#1209,.T.);
#3374=EDGE_CURVE('',#2664,#2663,#2087,.T.);
#3375=EDGE_CURVE('',#2662,#2664,#1210,.T.);
#3376=EDGE_CURVE('',#2665,#2666,#2088,.T.);
#3377=EDGE_CURVE('',#2667,#2665,#1211,.T.);
#3378=EDGE_CURVE('',#2668,#2667,#2089,.T.);
#3379=EDGE_CURVE('',#2666,#2668,#1212,.T.);
#3380=EDGE_CURVE('',#2669,#2670,#2090,.T.);
#3381=EDGE_CURVE('',#2671,#2669,#1213,.T.);
#3382=EDGE_CURVE('',#2672,#2671,#2091,.T.);
#3383=EDGE_CURVE('',#2670,#2672,#1214,.T.);
#3384=EDGE_CURVE('',#2673,#2674,#2092,.T.);
#3385=EDGE_CURVE('',#2675,#2673,#1215,.T.);
#3386=EDGE_CURVE('',#2676,#2675,#2093,.T.);
#3387=EDGE_CURVE('',#2674,#2676,#1216,.T.);
#3388=EDGE_CURVE('',#2677,#2678,#2094,.T.);
#3389=EDGE_CURVE('',#2679,#2677,#1217,.T.);
#3390=EDGE_CURVE('',#2680,#2679,#2095,.T.);
#3391=EDGE_CURVE('',#2678,#2680,#1218,.T.);
#3392=EDGE_CURVE('',#2681,#2682,#2096,.T.);
#3393=EDGE_CURVE('',#2683,#2681,#1219,.T.);
#3394=EDGE_CURVE('',#2684,#2683,#2097,.T.);
#3395=EDGE_CURVE('',#2682,#2684,#1220,.T.);
#3396=EDGE_CURVE('',#2685,#2686,#2098,.T.);
#3397=EDGE_CURVE('',#2687,#2685,#1221,.T.);
#3398=EDGE_CURVE('',#2688,#2687,#2099,.T.);
#3399=EDGE_CURVE('',#2686,#2688,#1222,.T.);
#3400=EDGE_CURVE('',#2689,#2690,#2100,.T.);
#3401=EDGE_CURVE('',#2691,#2689,#1223,.T.);
#3402=EDGE_CURVE('',#2692,#2691,#2101,.T.);
#3403=EDGE_CURVE('',#2690,#2692,#1224,.T.);
#3404=EDGE_CURVE('',#2693,#2694,#2102,.T.);
#3405=EDGE_CURVE('',#2693,#2695,#1225,.T.);
#3406=EDGE_CURVE('',#2695,#2696,#2103,.T.);
#3407=EDGE_CURVE('',#2696,#2694,#1226,.T.);
#3408=EDGE_CURVE('',#2697,#2698,#2104,.T.);
#3409=EDGE_CURVE('',#2697,#2699,#1227,.T.);
#3410=EDGE_CURVE('',#2699,#2700,#2105,.T.);
#3411=EDGE_CURVE('',#2700,#2698,#1228,.T.);
#3412=EDGE_CURVE('',#2701,#2702,#2106,.T.);
#3413=EDGE_CURVE('',#2702,#2703,#1229,.T.);
#3414=EDGE_CURVE('',#2704,#2703,#2107,.T.);
#3415=EDGE_CURVE('',#2704,#2701,#1230,.T.);
#3416=EDGE_CURVE('',#2705,#2706,#2108,.T.);
#3417=EDGE_CURVE('',#2705,#2707,#1231,.T.);
#3418=EDGE_CURVE('',#2707,#2708,#2109,.T.);
#3419=EDGE_CURVE('',#2708,#2706,#1232,.T.);
#3420=EDGE_CURVE('',#2709,#2710,#2110,.T.);
#3421=EDGE_CURVE('',#2709,#2711,#1233,.T.);
#3422=EDGE_CURVE('',#2711,#2712,#2111,.T.);
#3423=EDGE_CURVE('',#2712,#2710,#1234,.T.);
#3424=EDGE_CURVE('',#2713,#2714,#2112,.T.);
#3425=EDGE_CURVE('',#2714,#2715,#1235,.T.);
#3426=EDGE_CURVE('',#2716,#2715,#2113,.T.);
#3427=EDGE_CURVE('',#2716,#2713,#1236,.T.);
#3428=EDGE_CURVE('',#2717,#2718,#2114,.T.);
#3429=EDGE_CURVE('',#2718,#2719,#1237,.T.);
#3430=EDGE_CURVE('',#2720,#2719,#2115,.T.);
#3431=EDGE_CURVE('',#2720,#2717,#1238,.T.);
#3432=EDGE_CURVE('',#2721,#2722,#2116,.T.);
#3433=EDGE_CURVE('',#2722,#2723,#1239,.T.);
#3434=EDGE_CURVE('',#2724,#2723,#2117,.T.);
#3435=EDGE_CURVE('',#2724,#2721,#1240,.T.);
#3436=EDGE_CURVE('',#2725,#2726,#2118,.T.);
#3437=EDGE_CURVE('',#2725,#2727,#1241,.T.);
#3438=EDGE_CURVE('',#2727,#2728,#2119,.T.);
#3439=EDGE_CURVE('',#2728,#2726,#1242,.T.);
#3440=EDGE_CURVE('',#2729,#2730,#2120,.T.);
#3441=EDGE_CURVE('',#2729,#2731,#1243,.T.);
#3442=EDGE_CURVE('',#2731,#2732,#2121,.T.);
#3443=EDGE_CURVE('',#2732,#2730,#1244,.T.);
#3444=EDGE_CURVE('',#2733,#2734,#2122,.T.);
#3445=EDGE_CURVE('',#2734,#2735,#1245,.T.);
#3446=EDGE_CURVE('',#2736,#2735,#2123,.T.);
#3447=EDGE_CURVE('',#2736,#2733,#1246,.T.);
#3448=EDGE_CURVE('',#2737,#2738,#2124,.T.);
#3449=EDGE_CURVE('',#2738,#2739,#1247,.T.);
#3450=EDGE_CURVE('',#2740,#2739,#2125,.T.);
#3451=EDGE_CURVE('',#2740,#2737,#1248,.T.);
#3452=EDGE_CURVE('',#2741,#2742,#2126,.T.);
#3453=EDGE_CURVE('',#2742,#2743,#1249,.T.);
#3454=EDGE_CURVE('',#2744,#2743,#2127,.T.);
#3455=EDGE_CURVE('',#2744,#2741,#1250,.T.);
#3456=EDGE_CURVE('',#2745,#2746,#2128,.T.);
#3457=EDGE_CURVE('',#2746,#2747,#1251,.T.);
#3458=EDGE_CURVE('',#2748,#2747,#2129,.T.);
#3459=EDGE_CURVE('',#2748,#2745,#1252,.T.);
#3460=EDGE_CURVE('',#2633,#2749,#2130,.T.);
#3461=EDGE_CURVE('',#2749,#2750,#1253,.T.);
#3462=EDGE_CURVE('',#2634,#2750,#2131,.T.);
#3463=EDGE_CURVE('',#2639,#2751,#2132,.T.);
#3464=EDGE_CURVE('',#2751,#2752,#1254,.T.);
#3465=EDGE_CURVE('',#2640,#2752,#2133,.T.);
#3466=EDGE_CURVE('',#2753,#2652,#2134,.T.);
#3467=EDGE_CURVE('',#2753,#2754,#1255,.T.);
#3468=EDGE_CURVE('',#2754,#2651,#2135,.T.);
#3469=EDGE_CURVE('',#2755,#2756,#2136,.T.);
#3470=EDGE_CURVE('',#2755,#2757,#1256,.T.);
#3471=EDGE_CURVE('',#2757,#2758,#2137,.T.);
#3472=EDGE_CURVE('',#2758,#2756,#1257,.T.);
#3473=EDGE_CURVE('',#2759,#2760,#2138,.T.);
#3474=EDGE_CURVE('',#2759,#2761,#1258,.T.);
#3475=EDGE_CURVE('',#2761,#2762,#2139,.T.);
#3476=EDGE_CURVE('',#2762,#2760,#1259,.T.);
#3477=EDGE_CURVE('',#2763,#2764,#2140,.T.);
#3478=EDGE_CURVE('',#2764,#2765,#1260,.T.);
#3479=EDGE_CURVE('',#2766,#2765,#2141,.T.);
#3480=EDGE_CURVE('',#2766,#2763,#1261,.T.);
#3481=EDGE_CURVE('',#2767,#2768,#2142,.T.);
#3482=EDGE_CURVE('',#2767,#2769,#1262,.T.);
#3483=EDGE_CURVE('',#2769,#2770,#2143,.T.);
#3484=EDGE_CURVE('',#2770,#2768,#1263,.T.);
#3485=EDGE_CURVE('',#2771,#2772,#2144,.T.);
#3486=EDGE_CURVE('',#2771,#2773,#1264,.T.);
#3487=EDGE_CURVE('',#2773,#2774,#2145,.T.);
#3488=EDGE_CURVE('',#2774,#2772,#1265,.T.);
#3489=EDGE_CURVE('',#2775,#2776,#2146,.T.);
#3490=EDGE_CURVE('',#2775,#2777,#1266,.T.);
#3491=EDGE_CURVE('',#2777,#2778,#2147,.T.);
#3492=EDGE_CURVE('',#2778,#2776,#1267,.T.);
#3493=EDGE_CURVE('',#2779,#2780,#2148,.T.);
#3494=EDGE_CURVE('',#2779,#2781,#1268,.T.);
#3495=EDGE_CURVE('',#2781,#2782,#2149,.T.);
#3496=EDGE_CURVE('',#2782,#2780,#1269,.T.);
#3497=EDGE_CURVE('',#2783,#2784,#2150,.T.);
#3498=EDGE_CURVE('',#2783,#2785,#1270,.T.);
#3499=EDGE_CURVE('',#2785,#2786,#2151,.T.);
#3500=EDGE_CURVE('',#2786,#2784,#1271,.T.);
#3501=EDGE_CURVE('',#2787,#2788,#2152,.T.);
#3502=EDGE_CURVE('',#2788,#2789,#1272,.T.);
#3503=EDGE_CURVE('',#2790,#2789,#2153,.T.);
#3504=EDGE_CURVE('',#2790,#2787,#1273,.T.);
#3505=EDGE_CURVE('',#2791,#2792,#2154,.T.);
#3506=EDGE_CURVE('',#2792,#2793,#1274,.T.);
#3507=EDGE_CURVE('',#2794,#2793,#2155,.T.);
#3508=EDGE_CURVE('',#2794,#2791,#1275,.T.);
#3509=EDGE_CURVE('',#2795,#2796,#2156,.T.);
#3510=EDGE_CURVE('',#2796,#2797,#1276,.T.);
#3511=EDGE_CURVE('',#2798,#2797,#2157,.T.);
#3512=EDGE_CURVE('',#2798,#2795,#1277,.T.);
#3513=EDGE_CURVE('',#2799,#2800,#2158,.T.);
#3514=EDGE_CURVE('',#2799,#2801,#1278,.T.);
#3515=EDGE_CURVE('',#2801,#2802,#2159,.T.);
#3516=EDGE_CURVE('',#2802,#2800,#1279,.T.);
#3517=EDGE_CURVE('',#2699,#2803,#2160,.T.);
#3518=EDGE_CURVE('',#2803,#2804,#2161,.T.);
#3519=EDGE_CURVE('',#2804,#2805,#2162,.T.);
#3520=EDGE_CURVE('',#2805,#2806,#2163,.T.);
#3521=EDGE_CURVE('',#2806,#2702,#2164,.T.);
#3522=EDGE_CURVE('',#2701,#2807,#2165,.T.);
#3523=EDGE_CURVE('',#2807,#2808,#2166,.T.);
#3524=EDGE_CURVE('',#2808,#2809,#2167,.T.);
#3525=EDGE_CURVE('',#2809,#2810,#2168,.T.);
#3526=EDGE_CURVE('',#2810,#2714,#2169,.T.);
#3527=EDGE_CURVE('',#2713,#2811,#2170,.T.);
#3528=EDGE_CURVE('',#2811,#2812,#2171,.T.);
#3529=EDGE_CURVE('',#2812,#2813,#2172,.T.);
#3530=EDGE_CURVE('',#2813,#2814,#2173,.T.);
#3531=EDGE_CURVE('',#2814,#2718,#2174,.T.);
#3532=EDGE_CURVE('',#2717,#2815,#2175,.T.);
#3533=EDGE_CURVE('',#2815,#2816,#2176,.T.);
#3534=EDGE_CURVE('',#2816,#2817,#2177,.T.);
#3535=EDGE_CURVE('',#2817,#2818,#2178,.T.);
#3536=EDGE_CURVE('',#2818,#2696,#2179,.T.);
#3537=EDGE_CURVE('',#2695,#2819,#2180,.T.);
#3538=EDGE_CURVE('',#2819,#2820,#2181,.T.);
#3539=EDGE_CURVE('',#2820,#2821,#2182,.T.);
#3540=EDGE_CURVE('',#2821,#2822,#2183,.T.);
#3541=EDGE_CURVE('',#2822,#2722,#2184,.T.);
#3542=EDGE_CURVE('',#2721,#2823,#2185,.T.);
#3543=EDGE_CURVE('',#2823,#2824,#2186,.T.);
#3544=EDGE_CURVE('',#2824,#2825,#2187,.T.);
#3545=EDGE_CURVE('',#2825,#2826,#2188,.T.);
#3546=EDGE_CURVE('',#2826,#2734,#2189,.T.);
#3547=EDGE_CURVE('',#2733,#2827,#2190,.T.);
#3548=EDGE_CURVE('',#2827,#2828,#2191,.T.);
#3549=EDGE_CURVE('',#2828,#2829,#2192,.T.);
#3550=EDGE_CURVE('',#2829,#2830,#2193,.T.);
#3551=EDGE_CURVE('',#2830,#2738,#2194,.T.);
#3552=EDGE_CURVE('',#2737,#2831,#2195,.T.);
#3553=EDGE_CURVE('',#2831,#2832,#2196,.T.);
#3554=EDGE_CURVE('',#2832,#2833,#2197,.T.);
#3555=EDGE_CURVE('',#2833,#2834,#2198,.T.);
#3556=EDGE_CURVE('',#2834,#2732,#2199,.T.);
#3557=EDGE_CURVE('',#2731,#2835,#2200,.T.);
#3558=EDGE_CURVE('',#2835,#2836,#2201,.T.);
#3559=EDGE_CURVE('',#2836,#2837,#2202,.T.);
#3560=EDGE_CURVE('',#2837,#2838,#2203,.T.);
#3561=EDGE_CURVE('',#2838,#2728,#2204,.T.);
#3562=EDGE_CURVE('',#2727,#2839,#2205,.T.);
#3563=EDGE_CURVE('',#2839,#2840,#2206,.T.);
#3564=EDGE_CURVE('',#2840,#2841,#2207,.T.);
#3565=EDGE_CURVE('',#2841,#2842,#2208,.T.);
#3566=EDGE_CURVE('',#2842,#2742,#2209,.T.);
#3567=EDGE_CURVE('',#2741,#2843,#2210,.T.);
#3568=EDGE_CURVE('',#2843,#2844,#2211,.T.);
#3569=EDGE_CURVE('',#2844,#2845,#2212,.T.);
#3570=EDGE_CURVE('',#2845,#2846,#2213,.T.);
#3571=EDGE_CURVE('',#2846,#2746,#2214,.T.);
#3572=EDGE_CURVE('',#2745,#2847,#2215,.T.);
#3573=EDGE_CURVE('',#2847,#2848,#2216,.T.);
#3574=EDGE_CURVE('',#2848,#2849,#2217,.T.);
#3575=EDGE_CURVE('',#2849,#2850,#2218,.T.);
#3576=EDGE_CURVE('',#2850,#2749,#2219,.T.);
#3577=EDGE_CURVE('',#2631,#2851,#2220,.T.);
#3578=EDGE_CURVE('',#2851,#2852,#2221,.T.);
#3579=EDGE_CURVE('',#2852,#2751,#2222,.T.);
#3580=EDGE_CURVE('',#2637,#2853,#2223,.T.);
#3581=EDGE_CURVE('',#2853,#2854,#2224,.T.);
#3582=EDGE_CURVE('',#2854,#2788,#2225,.T.);
#3583=EDGE_CURVE('',#2787,#2684,#2226,.T.);
#3584=EDGE_CURVE('',#2683,#2855,#2227,.T.);
#3585=EDGE_CURVE('',#2855,#2856,#2228,.T.);
#3586=EDGE_CURVE('',#2856,#2786,#2229,.T.);
#3587=EDGE_CURVE('',#2785,#2680,#2230,.T.);
#3588=EDGE_CURVE('',#2679,#2857,#2231,.T.);
#3589=EDGE_CURVE('',#2857,#2858,#2232,.T.);
#3590=EDGE_CURVE('',#2858,#2792,#2233,.T.);
#3591=EDGE_CURVE('',#2791,#2688,#2234,.T.);
#3592=EDGE_CURVE('',#2687,#2859,#2235,.T.);
#3593=EDGE_CURVE('',#2859,#2860,#2236,.T.);
#3594=EDGE_CURVE('',#2860,#2796,#2237,.T.);
#3595=EDGE_CURVE('',#2795,#2692,#2238,.T.);
#3596=EDGE_CURVE('',#2691,#2861,#2239,.T.);
#3597=EDGE_CURVE('',#2861,#2862,#2240,.T.);
#3598=EDGE_CURVE('',#2862,#2782,#2241,.T.);
#3599=EDGE_CURVE('',#2781,#2676,#2242,.T.);
#3600=EDGE_CURVE('',#2675,#2863,#2243,.T.);
#3601=EDGE_CURVE('',#2863,#2864,#2244,.T.);
#3602=EDGE_CURVE('',#2864,#2778,#2245,.T.);
#3603=EDGE_CURVE('',#2777,#2865,#2246,.T.);
#3604=EDGE_CURVE('',#2865,#2866,#2247,.T.);
#3605=EDGE_CURVE('',#2866,#2672,#2248,.T.);
#3606=EDGE_CURVE('',#2671,#2774,#2249,.T.);
#3607=EDGE_CURVE('',#2773,#2867,#2250,.T.);
#3608=EDGE_CURVE('',#2867,#2868,#2251,.T.);
#3609=EDGE_CURVE('',#2868,#2668,#2252,.T.);
#3610=EDGE_CURVE('',#2667,#2770,#2253,.T.);
#3611=EDGE_CURVE('',#2769,#2869,#2254,.T.);
#3612=EDGE_CURVE('',#2869,#2870,#2255,.T.);
#3613=EDGE_CURVE('',#2870,#2664,#2256,.T.);
#3614=EDGE_CURVE('',#2663,#2762,#2257,.T.);
#3615=EDGE_CURVE('',#2761,#2871,#2258,.T.);
#3616=EDGE_CURVE('',#2871,#2872,#2259,.T.);
#3617=EDGE_CURVE('',#2872,#2656,#2260,.T.);
#3618=EDGE_CURVE('',#2655,#2764,#2261,.T.);
#3619=EDGE_CURVE('',#2763,#2873,#2262,.T.);
#3620=EDGE_CURVE('',#2873,#2874,#2263,.T.);
#3621=EDGE_CURVE('',#2874,#2660,#2264,.T.);
#3622=EDGE_CURVE('',#2659,#2758,#2265,.T.);
#3623=EDGE_CURVE('',#2757,#2875,#2266,.T.);
#3624=EDGE_CURVE('',#2875,#2876,#2267,.T.);
#3625=EDGE_CURVE('',#2876,#2650,#2268,.T.);
#3626=EDGE_CURVE('',#2754,#2877,#2269,.T.);
#3627=EDGE_CURVE('',#2877,#2878,#2270,.T.);
#3628=EDGE_CURVE('',#2878,#2644,#2271,.T.);
#3629=EDGE_CURVE('',#2879,#2645,#2272,.T.);
#3630=EDGE_CURVE('',#2879,#2880,#2273,.T.);
#3631=EDGE_CURVE('',#2880,#2881,#2274,.T.);
#3632=EDGE_CURVE('',#2881,#2882,#2275,.T.);
#3633=EDGE_CURVE('',#2882,#2883,#2276,.T.);
#3634=EDGE_CURVE('',#2883,#2802,#2277,.T.);
#3635=EDGE_CURVE('',#2801,#2884,#2278,.T.);
#3636=EDGE_CURVE('',#2884,#2885,#2279,.T.);
#3637=EDGE_CURVE('',#2885,#2886,#2280,.T.);
#3638=EDGE_CURVE('',#2886,#2887,#2281,.T.);
#3639=EDGE_CURVE('',#2887,#2712,#2282,.T.);
#3640=EDGE_CURVE('',#2711,#2888,#2283,.T.);
#3641=EDGE_CURVE('',#2888,#2889,#2284,.T.);
#3642=EDGE_CURVE('',#2889,#2890,#2285,.T.);
#3643=EDGE_CURVE('',#2890,#2891,#2286,.T.);
#3644=EDGE_CURVE('',#2891,#2708,#2287,.T.);
#3645=EDGE_CURVE('',#2707,#2892,#2288,.T.);
#3646=EDGE_CURVE('',#2892,#2893,#2289,.T.);
#3647=EDGE_CURVE('',#2893,#2894,#2290,.T.);
#3648=EDGE_CURVE('',#2894,#2895,#2291,.T.);
#3649=EDGE_CURVE('',#2895,#2700,#2292,.T.);
#3650=EDGE_CURVE('',#2896,#2625,#1280,.T.);
#3651=EDGE_CURVE('',#2626,#2897,#1281,.T.);
#3652=EDGE_CURVE('',#2897,#2896,#1282,.T.);
#3653=EDGE_CURVE('',#2697,#2898,#2293,.T.);
#3654=EDGE_CURVE('',#2899,#2698,#2294,.T.);
#3655=EDGE_CURVE('',#2899,#2900,#2295,.T.);
#3656=EDGE_CURVE('',#2901,#2900,#2296,.T.);
#3657=EDGE_CURVE('',#2901,#2902,#2297,.T.);
#3658=EDGE_CURVE('',#2705,#2902,#2298,.T.);
#3659=EDGE_CURVE('',#2903,#2706,#2299,.T.);
#3660=EDGE_CURVE('',#2903,#2904,#2300,.T.);
#3661=EDGE_CURVE('',#2905,#2904,#2301,.T.);
#3662=EDGE_CURVE('',#2905,#2906,#2302,.T.);
#3663=EDGE_CURVE('',#2709,#2906,#2303,.T.);
#3664=EDGE_CURVE('',#2907,#2710,#2304,.T.);
#3665=EDGE_CURVE('',#2907,#2908,#2305,.T.);
#3666=EDGE_CURVE('',#2909,#2908,#2306,.T.);
#3667=EDGE_CURVE('',#2909,#2910,#2307,.T.);
#3668=EDGE_CURVE('',#2799,#2910,#2308,.T.);
#3669=EDGE_CURVE('',#2911,#2800,#2309,.T.);
#3670=EDGE_CURVE('',#2911,#2912,#2310,.T.);
#3671=EDGE_CURVE('',#2913,#2912,#2311,.T.);
#3672=EDGE_CURVE('',#2913,#2914,#2312,.T.);
#3673=EDGE_CURVE('',#2915,#2914,#2313,.T.);
#3674=EDGE_CURVE('',#2915,#2646,#2314,.T.);
#3675=EDGE_CURVE('',#2916,#2642,#2315,.T.);
#3676=EDGE_CURVE('',#2916,#2917,#2316,.T.);
#3677=EDGE_CURVE('',#2753,#2917,#2317,.T.);
#3678=EDGE_CURVE('',#2918,#2648,#2318,.T.);
#3679=EDGE_CURVE('',#2918,#2919,#2319,.T.);
#3680=EDGE_CURVE('',#2755,#2919,#2320,.T.);
#3681=EDGE_CURVE('',#2657,#2756,#2321,.T.);
#3682=EDGE_CURVE('',#2920,#2658,#2322,.T.);
#3683=EDGE_CURVE('',#2920,#2921,#2323,.T.);
#3684=EDGE_CURVE('',#2766,#2921,#2324,.T.);
#3685=EDGE_CURVE('',#2653,#2765,#2325,.T.);
#3686=EDGE_CURVE('',#2922,#2654,#2326,.T.);
#3687=EDGE_CURVE('',#2922,#2923,#2327,.T.);
#3688=EDGE_CURVE('',#2759,#2923,#2328,.T.);
#3689=EDGE_CURVE('',#2661,#2760,#2329,.T.);
#3690=EDGE_CURVE('',#2924,#2662,#2330,.T.);
#3691=EDGE_CURVE('',#2924,#2925,#2331,.T.);
#3692=EDGE_CURVE('',#2767,#2925,#2332,.T.);
#3693=EDGE_CURVE('',#2665,#2768,#2333,.T.);
#3694=EDGE_CURVE('',#2926,#2666,#2334,.T.);
#3695=EDGE_CURVE('',#2926,#2927,#2335,.T.);
#3696=EDGE_CURVE('',#2771,#2927,#2336,.T.);
#3697=EDGE_CURVE('',#2669,#2772,#2337,.T.);
#3698=EDGE_CURVE('',#2928,#2670,#2338,.T.);
#3699=EDGE_CURVE('',#2928,#2929,#2339,.T.);
#3700=EDGE_CURVE('',#2775,#2929,#2340,.T.);
#3701=EDGE_CURVE('',#2930,#2776,#2341,.T.);
#3702=EDGE_CURVE('',#2930,#2931,#2342,.T.);
#3703=EDGE_CURVE('',#2673,#2931,#2343,.T.);
#3704=EDGE_CURVE('',#2779,#2674,#2344,.T.);
#3705=EDGE_CURVE('',#2932,#2780,#2345,.T.);
#3706=EDGE_CURVE('',#2932,#2933,#2346,.T.);
#3707=EDGE_CURVE('',#2689,#2933,#2347,.T.);
#3708=EDGE_CURVE('',#2798,#2690,#2348,.T.);
#3709=EDGE_CURVE('',#2934,#2797,#2349,.T.);
#3710=EDGE_CURVE('',#2934,#2935,#2350,.T.);
#3711=EDGE_CURVE('',#2685,#2935,#2351,.T.);
#3712=EDGE_CURVE('',#2794,#2686,#2352,.T.);
#3713=EDGE_CURVE('',#2936,#2793,#2353,.T.);
#3714=EDGE_CURVE('',#2936,#2937,#2354,.T.);
#3715=EDGE_CURVE('',#2677,#2937,#2355,.T.);
#3716=EDGE_CURVE('',#2783,#2678,#2356,.T.);
#3717=EDGE_CURVE('',#2938,#2784,#2357,.T.);
#3718=EDGE_CURVE('',#2938,#2939,#2358,.T.);
#3719=EDGE_CURVE('',#2681,#2939,#2359,.T.);
#3720=EDGE_CURVE('',#2790,#2682,#2360,.T.);
#3721=EDGE_CURVE('',#2940,#2789,#2361,.T.);
#3722=EDGE_CURVE('',#2940,#2941,#2362,.T.);
#3723=EDGE_CURVE('',#2635,#2941,#2363,.T.);
#3724=EDGE_CURVE('',#2942,#2752,#2364,.T.);
#3725=EDGE_CURVE('',#2942,#2943,#2365,.T.);
#3726=EDGE_CURVE('',#2629,#2943,#2366,.T.);
#3727=EDGE_CURVE('',#2944,#2750,#2367,.T.);
#3728=EDGE_CURVE('',#2944,#2945,#2368,.T.);
#3729=EDGE_CURVE('',#2946,#2945,#2369,.T.);
#3730=EDGE_CURVE('',#2946,#2947,#2370,.T.);
#3731=EDGE_CURVE('',#2748,#2947,#2371,.T.);
#3732=EDGE_CURVE('',#2948,#2747,#2372,.T.);
#3733=EDGE_CURVE('',#2948,#2949,#2373,.T.);
#3734=EDGE_CURVE('',#2950,#2949,#2374,.T.);
#3735=EDGE_CURVE('',#2950,#2951,#2375,.T.);
#3736=EDGE_CURVE('',#2744,#2951,#2376,.T.);
#3737=EDGE_CURVE('',#2952,#2743,#2377,.T.);
#3738=EDGE_CURVE('',#2952,#2953,#2378,.T.);
#3739=EDGE_CURVE('',#2954,#2953,#2379,.T.);
#3740=EDGE_CURVE('',#2954,#2955,#2380,.T.);
#3741=EDGE_CURVE('',#2725,#2955,#2381,.T.);
#3742=EDGE_CURVE('',#2956,#2726,#2382,.T.);
#3743=EDGE_CURVE('',#2956,#2957,#2383,.T.);
#3744=EDGE_CURVE('',#2958,#2957,#2384,.T.);
#3745=EDGE_CURVE('',#2958,#2959,#2385,.T.);
#3746=EDGE_CURVE('',#2729,#2959,#2386,.T.);
#3747=EDGE_CURVE('',#2960,#2730,#2387,.T.);
#3748=EDGE_CURVE('',#2960,#2961,#2388,.T.);
#3749=EDGE_CURVE('',#2962,#2961,#2389,.T.);
#3750=EDGE_CURVE('',#2962,#2963,#2390,.T.);
#3751=EDGE_CURVE('',#2740,#2963,#2391,.T.);
#3752=EDGE_CURVE('',#2964,#2739,#2392,.T.);
#3753=EDGE_CURVE('',#2964,#2965,#2393,.T.);
#3754=EDGE_CURVE('',#2966,#2965,#2394,.T.);
#3755=EDGE_CURVE('',#2966,#2967,#2395,.T.);
#3756=EDGE_CURVE('',#2736,#2967,#2396,.T.);
#3757=EDGE_CURVE('',#2968,#2735,#2397,.T.);
#3758=EDGE_CURVE('',#2968,#2969,#2398,.T.);
#3759=EDGE_CURVE('',#2970,#2969,#2399,.T.);
#3760=EDGE_CURVE('',#2970,#2971,#2400,.T.);
#3761=EDGE_CURVE('',#2724,#2971,#2401,.T.);
#3762=EDGE_CURVE('',#2972,#2723,#2402,.T.);
#3763=EDGE_CURVE('',#2972,#2973,#2403,.T.);
#3764=EDGE_CURVE('',#2974,#2973,#2404,.T.);
#3765=EDGE_CURVE('',#2974,#2975,#2405,.T.);
#3766=EDGE_CURVE('',#2693,#2975,#2406,.T.);
#3767=EDGE_CURVE('',#2976,#2694,#2407,.T.);
#3768=EDGE_CURVE('',#2976,#2977,#2408,.T.);
#3769=EDGE_CURVE('',#2978,#2977,#2409,.T.);
#3770=EDGE_CURVE('',#2978,#2979,#2410,.T.);
#3771=EDGE_CURVE('',#2720,#2979,#2411,.T.);
#3772=EDGE_CURVE('',#2980,#2719,#2412,.T.);
#3773=EDGE_CURVE('',#2980,#2981,#2413,.T.);
#3774=EDGE_CURVE('',#2982,#2981,#2414,.T.);
#3775=EDGE_CURVE('',#2982,#2983,#2415,.T.);
#3776=EDGE_CURVE('',#2716,#2983,#2416,.T.);
#3777=EDGE_CURVE('',#2984,#2715,#2417,.T.);
#3778=EDGE_CURVE('',#2984,#2985,#2418,.T.);
#3779=EDGE_CURVE('',#2986,#2985,#2419,.T.);
#3780=EDGE_CURVE('',#2986,#2987,#2420,.T.);
#3781=EDGE_CURVE('',#2704,#2987,#2421,.T.);
#3782=EDGE_CURVE('',#2988,#2703,#2422,.T.);
#3783=EDGE_CURVE('',#2988,#2989,#2423,.T.);
#3784=EDGE_CURVE('',#2990,#2989,#2424,.T.);
#3785=EDGE_CURVE('',#2990,#2898,#2425,.T.);
#3786=EDGE_CURVE('',#2991,#2627,#1283,.T.);
#3787=EDGE_CURVE('',#2992,#2991,#1284,.T.);
#3788=EDGE_CURVE('',#2628,#2992,#1285,.T.);
#3789=EDGE_CURVE('',#2915,#2879,#1286,.T.);
#3790=EDGE_CURVE('',#2883,#2911,#1287,.T.);
#3791=EDGE_CURVE('',#2914,#2880,#1288,.T.);
#3792=EDGE_CURVE('',#2912,#2882,#1289,.T.);
#3793=EDGE_CURVE('',#2881,#2913,#1290,.T.);
#3794=EDGE_CURVE('',#2910,#2884,#1291,.T.);
#3795=EDGE_CURVE('',#2887,#2907,#1292,.T.);
#3796=EDGE_CURVE('',#2908,#2886,#1293,.T.);
#3797=EDGE_CURVE('',#2885,#2909,#1294,.T.);
#3798=EDGE_CURVE('',#2862,#2932,#1295,.T.);
#3799=EDGE_CURVE('',#2933,#2861,#1296,.T.);
#3800=EDGE_CURVE('',#2860,#2934,#1297,.T.);
#3801=EDGE_CURVE('',#2935,#2859,#1298,.T.);
#3802=EDGE_CURVE('',#2856,#2938,#1299,.T.);
#3803=EDGE_CURVE('',#2939,#2855,#1300,.T.);
#3804=EDGE_CURVE('',#2858,#2936,#1301,.T.);
#3805=EDGE_CURVE('',#2937,#2857,#1302,.T.);
#3806=EDGE_CURVE('',#2864,#2930,#1303,.T.);
#3807=EDGE_CURVE('',#2931,#2863,#1304,.T.);
#3808=EDGE_CURVE('',#2929,#2865,#1305,.T.);
#3809=EDGE_CURVE('',#2866,#2928,#1306,.T.);
#3810=EDGE_CURVE('',#2927,#2867,#1307,.T.);
#3811=EDGE_CURVE('',#2868,#2926,#1308,.T.);
#3812=EDGE_CURVE('',#2925,#2869,#1309,.T.);
#3813=EDGE_CURVE('',#2870,#2924,#1310,.T.);
#3814=EDGE_CURVE('',#2921,#2873,#1311,.T.);
#3815=EDGE_CURVE('',#2874,#2920,#1312,.T.);
#3816=EDGE_CURVE('',#2923,#2871,#1313,.T.);
#3817=EDGE_CURVE('',#2872,#2922,#1314,.T.);
#3818=EDGE_CURVE('',#2919,#2875,#1315,.T.);
#3819=EDGE_CURVE('',#2876,#2918,#1316,.T.);
#3820=EDGE_CURVE('',#2917,#2877,#1317,.T.);
#3821=EDGE_CURVE('',#2878,#2916,#1318,.T.);
#3822=EDGE_CURVE('',#2854,#2940,#1319,.T.);
#3823=EDGE_CURVE('',#2941,#2853,#1320,.T.);
#3824=EDGE_CURVE('',#2852,#2942,#1321,.T.);
#3825=EDGE_CURVE('',#2943,#2851,#1322,.T.);
#3826=EDGE_CURVE('',#2947,#2847,#1323,.T.);
#3827=EDGE_CURVE('',#2850,#2944,#1324,.T.);
#3828=EDGE_CURVE('',#2945,#2849,#1325,.T.);
#3829=EDGE_CURVE('',#2848,#2946,#1326,.T.);
#3830=EDGE_CURVE('',#2951,#2843,#1327,.T.);
#3831=EDGE_CURVE('',#2846,#2948,#1328,.T.);
#3832=EDGE_CURVE('',#2949,#2845,#1329,.T.);
#3833=EDGE_CURVE('',#2844,#2950,#1330,.T.);
#3834=EDGE_CURVE('',#2963,#2831,#1331,.T.);
#3835=EDGE_CURVE('',#2834,#2960,#1332,.T.);
#3836=EDGE_CURVE('',#2961,#2833,#1333,.T.);
#3837=EDGE_CURVE('',#2832,#2962,#1334,.T.);
#3838=EDGE_CURVE('',#2967,#2827,#1335,.T.);
#3839=EDGE_CURVE('',#2830,#2964,#1336,.T.);
#3840=EDGE_CURVE('',#2965,#2829,#1337,.T.);
#3841=EDGE_CURVE('',#2828,#2966,#1338,.T.);
#3842=EDGE_CURVE('',#2959,#2835,#1339,.T.);
#3843=EDGE_CURVE('',#2838,#2956,#1340,.T.);
#3844=EDGE_CURVE('',#2957,#2837,#1341,.T.);
#3845=EDGE_CURVE('',#2836,#2958,#1342,.T.);
#3846=EDGE_CURVE('',#2955,#2839,#1343,.T.);
#3847=EDGE_CURVE('',#2842,#2952,#1344,.T.);
#3848=EDGE_CURVE('',#2953,#2841,#1345,.T.);
#3849=EDGE_CURVE('',#2840,#2954,#1346,.T.);
#3850=EDGE_CURVE('',#2971,#2823,#1347,.T.);
#3851=EDGE_CURVE('',#2826,#2968,#1348,.T.);
#3852=EDGE_CURVE('',#2969,#2825,#1349,.T.);
#3853=EDGE_CURVE('',#2824,#2970,#1350,.T.);
#3854=EDGE_CURVE('',#2975,#2819,#1351,.T.);
#3855=EDGE_CURVE('',#2822,#2972,#1352,.T.);
#3856=EDGE_CURVE('',#2973,#2821,#1353,.T.);
#3857=EDGE_CURVE('',#2820,#2974,#1354,.T.);
#3858=EDGE_CURVE('',#2979,#2815,#1355,.T.);
#3859=EDGE_CURVE('',#2818,#2976,#1356,.T.);
#3860=EDGE_CURVE('',#2977,#2817,#1357,.T.);
#3861=EDGE_CURVE('',#2816,#2978,#1358,.T.);
#3862=EDGE_CURVE('',#2983,#2811,#1359,.T.);
#3863=EDGE_CURVE('',#2814,#2980,#1360,.T.);
#3864=EDGE_CURVE('',#2981,#2813,#1361,.T.);
#3865=EDGE_CURVE('',#2812,#2982,#1362,.T.);
#3866=EDGE_CURVE('',#2906,#2888,#1363,.T.);
#3867=EDGE_CURVE('',#2891,#2903,#1364,.T.);
#3868=EDGE_CURVE('',#2904,#2890,#1365,.T.);
#3869=EDGE_CURVE('',#2889,#2905,#1366,.T.);
#3870=EDGE_CURVE('',#2902,#2892,#1367,.T.);
#3871=EDGE_CURVE('',#2895,#2899,#1368,.T.);
#3872=EDGE_CURVE('',#2900,#2894,#1369,.T.);
#3873=EDGE_CURVE('',#2893,#2901,#1370,.T.);
#3874=EDGE_CURVE('',#2987,#2807,#1371,.T.);
#3875=EDGE_CURVE('',#2810,#2984,#1372,.T.);
#3876=EDGE_CURVE('',#2985,#2809,#1373,.T.);
#3877=EDGE_CURVE('',#2808,#2986,#1374,.T.);
#3878=EDGE_CURVE('',#2898,#2803,#1375,.T.);
#3879=EDGE_CURVE('',#2806,#2988,#1376,.T.);
#3880=EDGE_CURVE('',#2989,#2805,#1377,.T.);
#3881=EDGE_CURVE('',#2804,#2990,#1378,.T.);
#3882=EDGE_CURVE('',#2896,#2991,#1379,.T.);
#3883=EDGE_CURVE('',#2897,#2992,#1380,.T.);
#3884=EDGE_CURVE('',#2993,#2993,#2426,.T.);
#3885=EDGE_CURVE('',#2993,#2994,#1381,.T.);
#3886=EDGE_CURVE('',#2994,#2994,#2427,.T.);
#3887=EDGE_CURVE('',#2995,#2996,#2428,.T.);
#3888=EDGE_CURVE('',#2995,#2997,#1382,.T.);
#3889=EDGE_CURVE('',#2997,#2998,#2429,.T.);
#3890=EDGE_CURVE('',#2998,#2999,#1383,.T.);
#3891=EDGE_CURVE('',#3000,#2999,#2430,.T.);
#3892=EDGE_CURVE('',#3001,#3000,#1384,.T.);
#3893=EDGE_CURVE('',#3001,#3002,#2431,.T.);
#3894=EDGE_CURVE('',#2996,#3002,#1385,.T.);
#3895=EDGE_CURVE('',#3003,#3003,#2432,.T.);
#3896=EDGE_CURVE('',#3003,#3004,#1386,.T.);
#3897=EDGE_CURVE('',#3004,#3004,#2433,.T.);
#3898=EDGE_CURVE('',#3005,#3006,#1387,.T.);
#3899=EDGE_CURVE('',#3006,#3007,#1388,.T.);
#3900=EDGE_CURVE('',#3007,#3008,#1389,.T.);
#3901=EDGE_CURVE('',#3008,#3009,#1390,.T.);
#3902=EDGE_CURVE('',#3009,#2995,#1391,.T.);
#3903=EDGE_CURVE('',#2996,#3010,#1392,.T.);
#3904=EDGE_CURVE('',#3010,#3011,#2434,.T.);
#3905=EDGE_CURVE('',#3011,#3012,#2435,.T.);
#3906=EDGE_CURVE('',#3012,#3013,#1393,.T.);
#3907=EDGE_CURVE('',#3013,#3005,#1394,.T.);
#3908=EDGE_CURVE('',#3014,#2997,#1395,.T.);
#3909=EDGE_CURVE('',#3014,#3015,#1396,.T.);
#3910=EDGE_CURVE('',#3016,#3015,#1397,.T.);
#3911=EDGE_CURVE('',#3017,#3016,#1398,.T.);
#3912=EDGE_CURVE('',#3017,#2998,#1399,.T.);
#3913=EDGE_CURVE('',#3018,#3019,#1400,.T.);
#3914=EDGE_CURVE('',#3020,#3018,#1401,.T.);
#3915=EDGE_CURVE('',#3021,#3020,#1402,.T.);
#3916=EDGE_CURVE('',#3022,#3021,#1403,.T.);
#3917=EDGE_CURVE('',#3022,#3023,#2436,.T.);
#3918=EDGE_CURVE('',#3024,#3023,#2437,.T.);
#3919=EDGE_CURVE('',#3002,#3024,#1404,.T.);
#3920=EDGE_CURVE('',#3025,#3001,#1405,.T.);
#3921=EDGE_CURVE('',#3026,#3025,#1406,.T.);
#3922=EDGE_CURVE('',#3019,#3026,#1407,.T.);
#3923=EDGE_CURVE('',#3027,#3028,#1408,.T.);
#3924=EDGE_CURVE('',#3028,#3000,#1409,.T.);
#3925=EDGE_CURVE('',#3029,#2999,#1410,.T.);
#3926=EDGE_CURVE('',#3029,#3030,#1411,.T.);
#3927=EDGE_CURVE('',#3030,#3027,#1412,.T.);
#3928=EDGE_CURVE('',#3009,#3014,#1413,.T.);
#3929=EDGE_CURVE('',#3025,#3028,#1414,.T.);
#3930=EDGE_CURVE('',#3010,#3024,#1415,.T.);
#3931=EDGE_CURVE('',#3017,#3029,#1416,.T.);
#3932=EDGE_CURVE('',#3023,#3011,#1417,.T.);
#3933=EDGE_CURVE('',#3012,#3022,#1418,.T.);
#3934=EDGE_CURVE('',#3013,#3021,#1419,.T.);
#3935=EDGE_CURVE('',#3005,#3020,#1420,.T.);
#3936=EDGE_CURVE('',#3031,#3018,#1421,.T.);
#3937=EDGE_CURVE('',#3031,#3032,#1422,.T.);
#3938=EDGE_CURVE('',#3033,#3032,#1423,.T.);
#3939=EDGE_CURVE('',#3034,#3033,#1424,.T.);
#3940=EDGE_CURVE('',#3034,#3006,#1425,.T.);
#3941=EDGE_CURVE('',#3032,#3035,#1426,.T.);
#3942=EDGE_CURVE('',#3036,#3035,#1427,.T.);
#3943=EDGE_CURVE('',#3033,#3036,#1428,.T.);
#3944=EDGE_CURVE('',#3008,#3015,#1429,.T.);
#3945=EDGE_CURVE('',#3037,#3007,#1430,.T.);
#3946=EDGE_CURVE('',#3036,#3037,#1431,.T.);
#3947=EDGE_CURVE('',#3035,#3038,#1432,.T.);
#3948=EDGE_CURVE('',#3038,#3019,#1433,.T.);
#3949=EDGE_CURVE('',#3026,#3027,#1434,.T.);
#3950=EDGE_CURVE('',#3016,#3030,#1435,.T.);
#3951=EDGE_CURVE('',#3034,#3037,#1436,.T.);
#3952=EDGE_CURVE('',#3031,#3038,#1437,.T.);
#3953=EDGE_CURVE('',#3039,#3039,#2438,.T.);
#3954=EDGE_CURVE('',#3039,#3040,#1438,.T.);
#3955=EDGE_CURVE('',#3041,#3040,#2439,.T.);
#3956=EDGE_CURVE('',#3041,#3042,#1439,.T.);
#3957=EDGE_CURVE('',#3042,#3043,#2440,.T.);
#3958=EDGE_CURVE('',#3044,#3043,#1440,.T.);
#3959=EDGE_CURVE('',#3045,#3044,#2441,.T.);
#3960=EDGE_CURVE('',#3045,#3046,#1441,.T.);
#3961=EDGE_CURVE('',#3046,#3047,#2442,.T.);
#3962=EDGE_CURVE('',#3048,#3047,#1442,.T.);
#3963=EDGE_CURVE('',#3040,#3048,#2443,.T.);
#3964=EDGE_CURVE('',#3049,#3049,#2444,.T.);
#3965=EDGE_CURVE('',#3049,#3050,#1443,.T.);
#3966=EDGE_CURVE('',#3050,#3050,#2445,.T.);
#3967=EDGE_CURVE('',#3044,#3051,#1444,.T.);
#3968=EDGE_CURVE('',#3052,#3051,#2446,.T.);
#3969=EDGE_CURVE('',#3052,#3045,#1445,.T.);
#3970=EDGE_CURVE('',#3051,#3053,#1446,.T.);
#3971=EDGE_CURVE('',#3054,#3053,#2447,.T.);
#3972=EDGE_CURVE('',#3052,#3054,#1447,.T.);
#3973=EDGE_CURVE('',#3055,#3056,#2448,.T.);
#3974=EDGE_CURVE('',#3056,#3057,#1448,.T.);
#3975=EDGE_CURVE('',#3057,#3058,#2449,.T.);
#3976=EDGE_CURVE('',#3058,#3055,#1449,.T.);
#3977=EDGE_CURVE('',#3059,#3060,#2450,.T.);
#3978=EDGE_CURVE('',#3056,#3060,#1450,.T.);
#3979=EDGE_CURVE('',#3055,#3059,#1451,.T.);
#3980=EDGE_CURVE('',#3060,#3061,#1452,.T.);
#3981=EDGE_CURVE('',#3057,#3061,#1453,.T.);
#3982=EDGE_CURVE('',#3061,#3062,#2451,.T.);
#3983=EDGE_CURVE('',#3058,#3062,#1454,.T.);
#3984=EDGE_CURVE('',#3062,#3059,#1455,.T.);
#3985=EDGE_CURVE('',#3063,#3064,#2452,.T.);
#3986=EDGE_CURVE('',#3063,#3041,#1456,.T.);
#3987=EDGE_CURVE('',#3048,#3064,#1457,.T.);
#3988=EDGE_CURVE('',#3065,#3066,#2453,.T.);
#3989=EDGE_CURVE('',#3063,#3065,#1458,.T.);
#3990=EDGE_CURVE('',#3064,#3066,#1459,.T.);
#3991=EDGE_CURVE('',#3043,#3053,#1460,.T.);
#3992=EDGE_CURVE('',#3065,#3042,#1461,.T.);
#3993=EDGE_CURVE('',#3047,#3066,#1462,.T.);
#3994=EDGE_CURVE('',#3054,#3046,#1463,.T.);
#3995=EDGE_CURVE('',#3067,#3068,#2454,.T.);
#3996=EDGE_CURVE('',#3068,#3069,#1464,.T.);
#3997=EDGE_CURVE('',#3070,#3069,#2455,.T.);
#3998=EDGE_CURVE('',#3067,#3070,#1465,.T.);
#3999=EDGE_CURVE('',#3071,#3072,#2456,.T.);
#4000=EDGE_CURVE('',#3071,#3073,#1466,.T.);
#4001=EDGE_CURVE('',#3073,#3074,#2457,.T.);
#4002=EDGE_CURVE('',#3072,#3074,#1467,.T.);
#4003=EDGE_CURVE('',#3075,#3075,#2458,.T.);
#4004=EDGE_CURVE('',#3075,#3076,#1468,.T.);
#4005=EDGE_CURVE('',#3076,#3076,#2459,.T.);
#4006=EDGE_CURVE('',#3077,#3077,#2460,.T.);
#4007=EDGE_CURVE('',#3077,#3078,#1469,.T.);
#4008=EDGE_CURVE('',#3078,#3078,#2461,.T.);
#4009=EDGE_CURVE('',#3079,#3080,#2462,.T.);
#4010=EDGE_CURVE('',#3079,#3081,#1470,.T.);
#4011=EDGE_CURVE('',#3081,#3082,#2463,.T.);
#4012=EDGE_CURVE('',#3080,#3082,#1471,.T.);
#4013=EDGE_CURVE('',#3083,#3081,#1472,.T.);
#4014=EDGE_CURVE('',#3084,#3083,#2464,.T.);
#4015=EDGE_CURVE('',#3082,#3084,#1473,.T.);
#4016=EDGE_CURVE('',#3085,#3086,#2465,.T.);
#4017=EDGE_CURVE('',#3086,#3070,#1474,.T.);
#4018=EDGE_CURVE('',#3069,#3085,#1475,.T.);
#4019=EDGE_CURVE('',#3087,#3079,#1476,.T.);
#4020=EDGE_CURVE('',#3087,#3083,#1477,.T.);
#4021=EDGE_CURVE('',#3088,#3084,#1478,.T.);
#4022=EDGE_CURVE('',#3080,#3088,#1479,.T.);
#4023=EDGE_CURVE('',#3088,#3087,#2466,.T.);
#4024=EDGE_CURVE('',#3089,#3073,#1480,.T.);
#4025=EDGE_CURVE('',#3090,#3089,#2467,.T.);
#4026=EDGE_CURVE('',#3074,#3090,#1481,.T.);
#4027=EDGE_CURVE('',#3091,#3071,#1482,.T.);
#4028=EDGE_CURVE('',#3091,#3089,#1483,.T.);
#4029=EDGE_CURVE('',#3092,#3091,#2468,.T.);
#4030=EDGE_CURVE('',#3092,#3090,#1484,.T.);
#4031=EDGE_CURVE('',#3072,#3092,#1485,.T.);
#4032=EDGE_CURVE('',#3093,#3085,#1486,.T.);
#4033=EDGE_CURVE('',#3093,#3094,#2469,.T.);
#4034=EDGE_CURVE('',#3094,#3086,#1487,.T.);
#4035=EDGE_CURVE('',#3094,#3067,#1488,.T.);
#4036=EDGE_CURVE('',#3068,#3093,#1489,.T.);
#4037=EDGE_CURVE('',#3095,#3095,#2470,.T.);
#4038=EDGE_CURVE('',#3095,#3096,#1490,.T.);
#4039=EDGE_CURVE('',#3097,#3096,#2471,.T.);
#4040=EDGE_CURVE('',#3097,#3098,#1491,.T.);
#4041=EDGE_CURVE('',#3098,#3099,#2472,.T.);
#4042=EDGE_CURVE('',#3100,#3099,#1492,.T.);
#4043=EDGE_CURVE('',#3101,#3100,#2473,.T.);
#4044=EDGE_CURVE('',#3101,#3102,#1493,.T.);
#4045=EDGE_CURVE('',#3102,#3103,#2474,.T.);
#4046=EDGE_CURVE('',#3104,#3103,#1494,.T.);
#4047=EDGE_CURVE('',#3096,#3104,#2475,.T.);
#4048=EDGE_CURVE('',#3105,#3105,#2476,.T.);
#4049=EDGE_CURVE('',#3105,#3106,#1495,.T.);
#4050=EDGE_CURVE('',#3106,#3106,#2477,.T.);
#4051=EDGE_CURVE('',#3100,#3107,#1496,.T.);
#4052=EDGE_CURVE('',#3108,#3107,#2478,.T.);
#4053=EDGE_CURVE('',#3108,#3101,#1497,.T.);
#4054=EDGE_CURVE('',#3107,#3109,#1498,.T.);
#4055=EDGE_CURVE('',#3110,#3109,#2479,.T.);
#4056=EDGE_CURVE('',#3108,#3110,#1499,.T.);
#4057=EDGE_CURVE('',#3111,#3112,#2480,.T.);
#4058=EDGE_CURVE('',#3111,#3097,#1500,.T.);
#4059=EDGE_CURVE('',#3104,#3112,#1501,.T.);
#4060=EDGE_CURVE('',#3113,#3114,#2481,.T.);
#4061=EDGE_CURVE('',#3111,#3113,#1502,.T.);
#4062=EDGE_CURVE('',#3112,#3114,#1503,.T.);
#4063=EDGE_CURVE('',#3099,#3109,#1504,.T.);
#4064=EDGE_CURVE('',#3113,#3098,#1505,.T.);
#4065=EDGE_CURVE('',#3103,#3114,#1506,.T.);
#4066=EDGE_CURVE('',#3110,#3102,#1507,.T.);
#4067=EDGE_CURVE('',#3115,#3116,#2482,.T.);
#4068=EDGE_CURVE('',#3117,#3115,#1508,.T.);
#4069=EDGE_CURVE('',#3118,#3117,#2483,.T.);
#4070=EDGE_CURVE('',#3116,#3118,#1509,.T.);
#4071=EDGE_CURVE('',#3119,#3116,#1510,.T.);
#4072=EDGE_CURVE('',#3120,#3119,#2484,.T.);
#4073=EDGE_CURVE('',#3120,#3115,#1511,.T.);
#4074=EDGE_CURVE('',#3121,#3118,#1512,.T.);
#4075=EDGE_CURVE('',#3119,#3121,#1513,.T.);
#4076=EDGE_CURVE('',#3122,#3117,#1514,.T.);
#4077=EDGE_CURVE('',#3121,#3122,#2485,.T.);
#4078=EDGE_CURVE('',#3122,#3120,#1515,.T.);
#4079=EDGE_CURVE('',#3123,#3124,#2486,.T.);
#4080=EDGE_CURVE('',#3124,#3123,#2487,.T.);
#4081=EDGE_CURVE('',#3124,#3125,#2488,.T.);
#4082=EDGE_CURVE('',#3125,#3125,#2489,.T.);
#4083=EDGE_CURVE('',#3126,#3127,#2490,.T.);
#4084=EDGE_CURVE('',#3127,#3128,#1516,.T.);
#4085=EDGE_CURVE('',#3129,#3128,#2491,.T.);
#4086=EDGE_CURVE('',#3126,#3129,#1517,.T.);
#4087=EDGE_CURVE('',#3123,#3130,#1518,.T.);
#4088=EDGE_CURVE('',#3130,#3130,#2492,.T.);
#4089=EDGE_CURVE('',#3131,#3132,#2493,.T.);
#4090=EDGE_CURVE('',#3133,#3132,#1519,.T.);
#4091=EDGE_CURVE('',#3133,#3134,#2494,.T.);
#4092=EDGE_CURVE('',#3134,#3135,#1520,.T.);
#4093=EDGE_CURVE('',#3135,#3135,#2495,.T.);
#4094=EDGE_CURVE('',#3134,#3136,#2496,.T.);
#4095=EDGE_CURVE('',#3136,#3137,#1521,.T.);
#4096=EDGE_CURVE('',#3137,#3138,#2497,.T.);
#4097=EDGE_CURVE('',#3139,#3138,#1522,.T.);
#4098=EDGE_CURVE('',#3139,#3140,#2498,.T.);
#4099=EDGE_CURVE('',#3140,#3131,#1523,.T.);
#4100=EDGE_CURVE('',#3137,#3141,#1524,.T.);
#4101=EDGE_CURVE('',#3141,#3142,#2499,.T.);
#4102=EDGE_CURVE('',#3142,#3138,#1525,.T.);
#4103=EDGE_CURVE('',#3131,#3129,#1526,.T.);
#4104=EDGE_CURVE('',#3128,#3132,#1527,.T.);
#4105=EDGE_CURVE('',#3143,#3139,#1528,.T.);
#4106=EDGE_CURVE('',#3144,#3143,#2500,.T.);
#4107=EDGE_CURVE('',#3136,#3144,#1529,.T.);
#4108=EDGE_CURVE('',#3127,#3133,#1530,.T.);
#4109=EDGE_CURVE('',#3140,#3126,#1531,.T.);
#4110=EDGE_CURVE('',#3144,#3141,#1532,.T.);
#4111=EDGE_CURVE('',#3143,#3142,#1533,.T.);
#4112=ORIENTED_EDGE('',*,*,#3145,.F.);
#4113=ORIENTED_EDGE('',*,*,#3146,.T.);
#4114=ORIENTED_EDGE('',*,*,#3147,.T.);
#4115=ORIENTED_EDGE('',*,*,#3146,.F.);
#4116=ORIENTED_EDGE('',*,*,#3148,.T.);
#4117=ORIENTED_EDGE('',*,*,#3149,.T.);
#4118=ORIENTED_EDGE('',*,*,#3150,.F.);
#4119=ORIENTED_EDGE('',*,*,#3149,.F.);
#4120=ORIENTED_EDGE('',*,*,#3151,.T.);
#4121=ORIENTED_EDGE('',*,*,#3152,.T.);
#4122=ORIENTED_EDGE('',*,*,#3153,.F.);
#4123=ORIENTED_EDGE('',*,*,#3152,.F.);
#4124=ORIENTED_EDGE('',*,*,#3154,.T.);
#4125=ORIENTED_EDGE('',*,*,#3155,.T.);
#4126=ORIENTED_EDGE('',*,*,#3156,.F.);
#4127=ORIENTED_EDGE('',*,*,#3155,.F.);
#4128=ORIENTED_EDGE('',*,*,#3157,.T.);
#4129=ORIENTED_EDGE('',*,*,#3158,.F.);
#4130=ORIENTED_EDGE('',*,*,#3159,.F.);
#4131=ORIENTED_EDGE('',*,*,#3160,.T.);
#4132=ORIENTED_EDGE('',*,*,#3161,.T.);
#4133=ORIENTED_EDGE('',*,*,#3162,.F.);
#4134=ORIENTED_EDGE('',*,*,#3163,.F.);
#4135=ORIENTED_EDGE('',*,*,#3158,.T.);
#4136=ORIENTED_EDGE('',*,*,#3164,.F.);
#4137=ORIENTED_EDGE('',*,*,#3165,.F.);
#4138=ORIENTED_EDGE('',*,*,#3166,.T.);
#4139=ORIENTED_EDGE('',*,*,#3162,.T.);
#4140=ORIENTED_EDGE('',*,*,#3167,.T.);
#4141=ORIENTED_EDGE('',*,*,#3168,.T.);
#4142=ORIENTED_EDGE('',*,*,#3169,.F.);
#4143=ORIENTED_EDGE('',*,*,#3165,.T.);
#4144=ORIENTED_EDGE('',*,*,#3170,.F.);
#4145=ORIENTED_EDGE('',*,*,#3171,.T.);
#4146=ORIENTED_EDGE('',*,*,#3172,.T.);
#4147=ORIENTED_EDGE('',*,*,#3173,.T.);
#4148=ORIENTED_EDGE('',*,*,#3174,.F.);
#4149=ORIENTED_EDGE('',*,*,#3175,.F.);
#4150=ORIENTED_EDGE('',*,*,#3176,.T.);
#4151=ORIENTED_EDGE('',*,*,#3177,.T.);
#4152=ORIENTED_EDGE('',*,*,#3178,.F.);
#4153=ORIENTED_EDGE('',*,*,#3179,.F.);
#4154=ORIENTED_EDGE('',*,*,#3180,.T.);
#4155=ORIENTED_EDGE('',*,*,#3175,.T.);
#4156=ORIENTED_EDGE('',*,*,#3181,.F.);
#4157=ORIENTED_EDGE('',*,*,#3182,.F.);
#4158=ORIENTED_EDGE('',*,*,#3183,.T.);
#4159=ORIENTED_EDGE('',*,*,#3179,.T.);
#4160=ORIENTED_EDGE('',*,*,#3184,.F.);
#4161=ORIENTED_EDGE('',*,*,#3185,.F.);
#4162=ORIENTED_EDGE('',*,*,#3186,.T.);
#4163=ORIENTED_EDGE('',*,*,#3187,.T.);
#4164=ORIENTED_EDGE('',*,*,#3188,.F.);
#4165=ORIENTED_EDGE('',*,*,#3189,.F.);
#4166=ORIENTED_EDGE('',*,*,#3190,.T.);
#4167=ORIENTED_EDGE('',*,*,#3185,.T.);
#4168=ORIENTED_EDGE('',*,*,#3191,.T.);
#4169=ORIENTED_EDGE('',*,*,#3192,.F.);
#4170=ORIENTED_EDGE('',*,*,#3193,.F.);
#4171=ORIENTED_EDGE('',*,*,#3189,.T.);
#4172=ORIENTED_EDGE('',*,*,#3194,.F.);
#4173=ORIENTED_EDGE('',*,*,#3195,.T.);
#4174=ORIENTED_EDGE('',*,*,#3196,.T.);
#4175=ORIENTED_EDGE('',*,*,#3160,.F.);
#4176=ORIENTED_EDGE('',*,*,#3197,.T.);
#4177=ORIENTED_EDGE('',*,*,#3177,.F.);
#4178=ORIENTED_EDGE('',*,*,#3198,.F.);
#4179=ORIENTED_EDGE('',*,*,#3182,.T.);
#4180=ORIENTED_EDGE('',*,*,#3199,.T.);
#4181=ORIENTED_EDGE('',*,*,#3187,.F.);
#4182=ORIENTED_EDGE('',*,*,#3200,.F.);
#4183=ORIENTED_EDGE('',*,*,#3192,.T.);
#4184=ORIENTED_EDGE('',*,*,#3169,.T.);
#4185=ORIENTED_EDGE('',*,*,#3201,.T.);
#4186=ORIENTED_EDGE('',*,*,#3170,.T.);
#4187=ORIENTED_EDGE('',*,*,#3202,.T.);
#4188=ORIENTED_EDGE('',*,*,#3194,.T.);
#4189=ORIENTED_EDGE('',*,*,#3159,.T.);
#4190=ORIENTED_EDGE('',*,*,#3163,.T.);
#4191=ORIENTED_EDGE('',*,*,#3166,.F.);
#4192=ORIENTED_EDGE('',*,*,#3154,.F.);
#4193=ORIENTED_EDGE('',*,*,#3145,.T.);
#4194=ORIENTED_EDGE('',*,*,#3148,.F.);
#4195=ORIENTED_EDGE('',*,*,#3151,.F.);
#4196=ORIENTED_EDGE('',*,*,#3186,.F.);
#4197=ORIENTED_EDGE('',*,*,#3190,.F.);
#4198=ORIENTED_EDGE('',*,*,#3193,.T.);
#4199=ORIENTED_EDGE('',*,*,#3200,.T.);
#4200=ORIENTED_EDGE('',*,*,#3176,.F.);
#4201=ORIENTED_EDGE('',*,*,#3180,.F.);
#4202=ORIENTED_EDGE('',*,*,#3183,.F.);
#4203=ORIENTED_EDGE('',*,*,#3198,.T.);
#4204=ORIENTED_EDGE('',*,*,#3172,.F.);
#4205=ORIENTED_EDGE('',*,*,#3203,.T.);
#4206=ORIENTED_EDGE('',*,*,#3167,.F.);
#4207=ORIENTED_EDGE('',*,*,#3164,.T.);
#4208=ORIENTED_EDGE('',*,*,#3161,.F.);
#4209=ORIENTED_EDGE('',*,*,#3157,.F.);
#4210=ORIENTED_EDGE('',*,*,#3196,.F.);
#4211=ORIENTED_EDGE('',*,*,#3204,.T.);
#4212=ORIENTED_EDGE('',*,*,#3156,.T.);
#4213=ORIENTED_EDGE('',*,*,#3147,.F.);
#4214=ORIENTED_EDGE('',*,*,#3150,.T.);
#4215=ORIENTED_EDGE('',*,*,#3153,.T.);
#4216=ORIENTED_EDGE('',*,*,#3184,.T.);
#4217=ORIENTED_EDGE('',*,*,#3199,.F.);
#4218=ORIENTED_EDGE('',*,*,#3191,.F.);
#4219=ORIENTED_EDGE('',*,*,#3188,.T.);
#4220=ORIENTED_EDGE('',*,*,#3174,.T.);
#4221=ORIENTED_EDGE('',*,*,#3197,.F.);
#4222=ORIENTED_EDGE('',*,*,#3181,.T.);
#4223=ORIENTED_EDGE('',*,*,#3178,.T.);
#4224=ORIENTED_EDGE('',*,*,#3201,.F.);
#4225=ORIENTED_EDGE('',*,*,#3168,.F.);
#4226=ORIENTED_EDGE('',*,*,#3203,.F.);
#4227=ORIENTED_EDGE('',*,*,#3171,.F.);
#4228=ORIENTED_EDGE('',*,*,#3202,.F.);
#4229=ORIENTED_EDGE('',*,*,#3173,.F.);
#4230=ORIENTED_EDGE('',*,*,#3204,.F.);
#4231=ORIENTED_EDGE('',*,*,#3195,.F.);
#4232=ORIENTED_EDGE('',*,*,#3205,.T.);
#4233=ORIENTED_EDGE('',*,*,#3206,.T.);
#4234=ORIENTED_EDGE('',*,*,#3207,.F.);
#4235=ORIENTED_EDGE('',*,*,#3206,.F.);
#4236=ORIENTED_EDGE('',*,*,#3208,.T.);
#4237=ORIENTED_EDGE('',*,*,#3209,.T.);
#4238=ORIENTED_EDGE('',*,*,#3210,.F.);
#4239=ORIENTED_EDGE('',*,*,#3211,.F.);
#4240=ORIENTED_EDGE('',*,*,#3212,.F.);
#4241=ORIENTED_EDGE('',*,*,#3213,.T.);
#4242=ORIENTED_EDGE('',*,*,#3214,.T.);
#4243=ORIENTED_EDGE('',*,*,#3215,.F.);
#4244=ORIENTED_EDGE('',*,*,#3216,.F.);
#4245=ORIENTED_EDGE('',*,*,#3217,.T.);
#4246=ORIENTED_EDGE('',*,*,#3218,.F.);
#4247=ORIENTED_EDGE('',*,*,#3217,.F.);
#4248=ORIENTED_EDGE('',*,*,#3219,.F.);
#4249=ORIENTED_EDGE('',*,*,#3220,.T.);
#4250=ORIENTED_EDGE('',*,*,#3221,.F.);
#4251=ORIENTED_EDGE('',*,*,#3220,.F.);
#4252=ORIENTED_EDGE('',*,*,#3222,.F.);
#4253=ORIENTED_EDGE('',*,*,#3223,.F.);
#4254=ORIENTED_EDGE('',*,*,#3224,.T.);
#4255=ORIENTED_EDGE('',*,*,#3225,.T.);
#4256=ORIENTED_EDGE('',*,*,#3226,.F.);
#4257=ORIENTED_EDGE('',*,*,#3227,.F.);
#4258=ORIENTED_EDGE('',*,*,#3228,.F.);
#4259=ORIENTED_EDGE('',*,*,#3229,.T.);
#4260=ORIENTED_EDGE('',*,*,#3227,.T.);
#4261=ORIENTED_EDGE('',*,*,#3230,.T.);
#4262=ORIENTED_EDGE('',*,*,#3231,.T.);
#4263=ORIENTED_EDGE('',*,*,#3232,.T.);
#4264=ORIENTED_EDGE('',*,*,#3223,.T.);
#4265=ORIENTED_EDGE('',*,*,#3233,.F.);
#4266=ORIENTED_EDGE('',*,*,#3234,.F.);
#4267=ORIENTED_EDGE('',*,*,#3235,.F.);
#4268=ORIENTED_EDGE('',*,*,#3214,.F.);
#4269=ORIENTED_EDGE('',*,*,#3236,.F.);
#4270=ORIENTED_EDGE('',*,*,#3205,.F.);
#4271=ORIENTED_EDGE('',*,*,#3225,.F.);
#4272=ORIENTED_EDGE('',*,*,#3237,.F.);
#4273=ORIENTED_EDGE('',*,*,#3238,.F.);
#4274=ORIENTED_EDGE('',*,*,#3239,.F.);
#4275=ORIENTED_EDGE('',*,*,#3221,.T.);
#4276=ORIENTED_EDGE('',*,*,#3210,.T.);
#4277=ORIENTED_EDGE('',*,*,#3240,.T.);
#4278=ORIENTED_EDGE('',*,*,#3241,.T.);
#4279=ORIENTED_EDGE('',*,*,#3242,.T.);
#4280=ORIENTED_EDGE('',*,*,#3218,.T.);
#4281=ORIENTED_EDGE('',*,*,#3239,.T.);
#4282=ORIENTED_EDGE('',*,*,#3243,.F.);
#4283=ORIENTED_EDGE('',*,*,#3230,.F.);
#4284=ORIENTED_EDGE('',*,*,#3226,.T.);
#4285=ORIENTED_EDGE('',*,*,#3238,.T.);
#4286=ORIENTED_EDGE('',*,*,#3244,.F.);
#4287=ORIENTED_EDGE('',*,*,#3231,.F.);
#4288=ORIENTED_EDGE('',*,*,#3243,.T.);
#4289=ORIENTED_EDGE('',*,*,#3237,.T.);
#4290=ORIENTED_EDGE('',*,*,#3224,.F.);
#4291=ORIENTED_EDGE('',*,*,#3232,.F.);
#4292=ORIENTED_EDGE('',*,*,#3244,.T.);
#4293=ORIENTED_EDGE('',*,*,#3234,.T.);
#4294=ORIENTED_EDGE('',*,*,#3245,.F.);
#4295=ORIENTED_EDGE('',*,*,#3246,.F.);
#4296=ORIENTED_EDGE('',*,*,#3247,.T.);
#4297=ORIENTED_EDGE('',*,*,#3235,.T.);
#4298=ORIENTED_EDGE('',*,*,#3247,.F.);
#4299=ORIENTED_EDGE('',*,*,#3248,.F.);
#4300=ORIENTED_EDGE('',*,*,#3215,.T.);
#4301=ORIENTED_EDGE('',*,*,#3236,.T.);
#4302=ORIENTED_EDGE('',*,*,#3213,.F.);
#4303=ORIENTED_EDGE('',*,*,#3249,.F.);
#4304=ORIENTED_EDGE('',*,*,#3245,.T.);
#4305=ORIENTED_EDGE('',*,*,#3246,.T.);
#4306=ORIENTED_EDGE('',*,*,#3249,.T.);
#4307=ORIENTED_EDGE('',*,*,#3212,.T.);
#4308=ORIENTED_EDGE('',*,*,#3248,.T.);
#4309=ORIENTED_EDGE('',*,*,#3240,.F.);
#4310=ORIENTED_EDGE('',*,*,#3209,.F.);
#4311=ORIENTED_EDGE('',*,*,#3250,.T.);
#4312=ORIENTED_EDGE('',*,*,#3251,.T.);
#4313=ORIENTED_EDGE('',*,*,#3241,.F.);
#4314=ORIENTED_EDGE('',*,*,#3251,.F.);
#4315=ORIENTED_EDGE('',*,*,#3252,.T.);
#4316=ORIENTED_EDGE('',*,*,#3253,.T.);
#4317=ORIENTED_EDGE('',*,*,#3242,.F.);
#4318=ORIENTED_EDGE('',*,*,#3253,.F.);
#4319=ORIENTED_EDGE('',*,*,#3254,.T.);
#4320=ORIENTED_EDGE('',*,*,#3211,.T.);
#4321=ORIENTED_EDGE('',*,*,#3208,.F.);
#4322=ORIENTED_EDGE('',*,*,#3254,.F.);
#4323=ORIENTED_EDGE('',*,*,#3252,.F.);
#4324=ORIENTED_EDGE('',*,*,#3250,.F.);
#4325=ORIENTED_EDGE('',*,*,#3255,.F.);
#4326=ORIENTED_EDGE('',*,*,#3222,.T.);
#4327=ORIENTED_EDGE('',*,*,#3256,.T.);
#4328=ORIENTED_EDGE('',*,*,#3257,.F.);
#4329=ORIENTED_EDGE('',*,*,#3229,.F.);
#4330=ORIENTED_EDGE('',*,*,#3258,.F.);
#4331=ORIENTED_EDGE('',*,*,#3259,.T.);
#4332=ORIENTED_EDGE('',*,*,#3260,.T.);
#4333=ORIENTED_EDGE('',*,*,#3256,.F.);
#4334=ORIENTED_EDGE('',*,*,#3228,.T.);
#4335=ORIENTED_EDGE('',*,*,#3261,.F.);
#4336=ORIENTED_EDGE('',*,*,#3262,.F.);
#4337=ORIENTED_EDGE('',*,*,#3258,.T.);
#4338=ORIENTED_EDGE('',*,*,#3233,.T.);
#4339=ORIENTED_EDGE('',*,*,#3255,.T.);
#4340=ORIENTED_EDGE('',*,*,#3263,.F.);
#4341=ORIENTED_EDGE('',*,*,#3264,.F.);
#4342=ORIENTED_EDGE('',*,*,#3261,.T.);
#4343=ORIENTED_EDGE('',*,*,#3257,.T.);
#4344=ORIENTED_EDGE('',*,*,#3260,.F.);
#4345=ORIENTED_EDGE('',*,*,#3265,.F.);
#4346=ORIENTED_EDGE('',*,*,#3263,.T.);
#4347=ORIENTED_EDGE('',*,*,#3259,.F.);
#4348=ORIENTED_EDGE('',*,*,#3262,.T.);
#4349=ORIENTED_EDGE('',*,*,#3264,.T.);
#4350=ORIENTED_EDGE('',*,*,#3265,.T.);
#4351=ORIENTED_EDGE('',*,*,#3219,.T.);
#4352=ORIENTED_EDGE('',*,*,#3207,.T.);
#4353=ORIENTED_EDGE('',*,*,#3216,.T.);
#4354=ORIENTED_EDGE('',*,*,#3266,.T.);
#4355=ORIENTED_EDGE('',*,*,#3267,.T.);
#4356=ORIENTED_EDGE('',*,*,#3268,.F.);
#4357=ORIENTED_EDGE('',*,*,#3267,.F.);
#4358=ORIENTED_EDGE('',*,*,#3269,.F.);
#4359=ORIENTED_EDGE('',*,*,#3270,.T.);
#4360=ORIENTED_EDGE('',*,*,#3271,.T.);
#4361=ORIENTED_EDGE('',*,*,#3272,.F.);
#4362=ORIENTED_EDGE('',*,*,#3273,.T.);
#4363=ORIENTED_EDGE('',*,*,#3274,.T.);
#4364=ORIENTED_EDGE('',*,*,#3275,.F.);
#4365=ORIENTED_EDGE('',*,*,#3274,.F.);
#4366=ORIENTED_EDGE('',*,*,#3276,.T.);
#4367=ORIENTED_EDGE('',*,*,#3277,.T.);
#4368=ORIENTED_EDGE('',*,*,#3278,.F.);
#4369=ORIENTED_EDGE('',*,*,#3279,.F.);
#4370=ORIENTED_EDGE('',*,*,#3280,.F.);
#4371=ORIENTED_EDGE('',*,*,#3281,.T.);
#4372=ORIENTED_EDGE('',*,*,#3282,.T.);
#4373=ORIENTED_EDGE('',*,*,#3283,.F.);
#4374=ORIENTED_EDGE('',*,*,#3284,.F.);
#4375=ORIENTED_EDGE('',*,*,#3285,.T.);
#4376=ORIENTED_EDGE('',*,*,#3286,.F.);
#4377=ORIENTED_EDGE('',*,*,#3285,.F.);
#4378=ORIENTED_EDGE('',*,*,#3287,.F.);
#4379=ORIENTED_EDGE('',*,*,#3288,.T.);
#4380=ORIENTED_EDGE('',*,*,#3289,.F.);
#4381=ORIENTED_EDGE('',*,*,#3288,.F.);
#4382=ORIENTED_EDGE('',*,*,#3290,.T.);
#4383=ORIENTED_EDGE('',*,*,#3291,.F.);
#4384=ORIENTED_EDGE('',*,*,#3292,.T.);
#4385=ORIENTED_EDGE('',*,*,#3269,.T.);
#4386=ORIENTED_EDGE('',*,*,#3266,.F.);
#4387=ORIENTED_EDGE('',*,*,#3293,.F.);
#4388=ORIENTED_EDGE('',*,*,#3294,.T.);
#4389=ORIENTED_EDGE('',*,*,#3295,.T.);
#4390=ORIENTED_EDGE('',*,*,#3296,.T.);
#4391=ORIENTED_EDGE('',*,*,#3297,.T.);
#4392=ORIENTED_EDGE('',*,*,#3298,.T.);
#4393=ORIENTED_EDGE('',*,*,#3299,.T.);
#4394=ORIENTED_EDGE('',*,*,#3300,.F.);
#4395=ORIENTED_EDGE('',*,*,#3301,.F.);
#4396=ORIENTED_EDGE('',*,*,#3302,.F.);
#4397=ORIENTED_EDGE('',*,*,#3282,.F.);
#4398=ORIENTED_EDGE('',*,*,#3303,.F.);
#4399=ORIENTED_EDGE('',*,*,#3273,.F.);
#4400=ORIENTED_EDGE('',*,*,#3304,.F.);
#4401=ORIENTED_EDGE('',*,*,#3271,.F.);
#4402=ORIENTED_EDGE('',*,*,#3305,.F.);
#4403=ORIENTED_EDGE('',*,*,#3306,.F.);
#4404=ORIENTED_EDGE('',*,*,#3289,.T.);
#4405=ORIENTED_EDGE('',*,*,#3278,.T.);
#4406=ORIENTED_EDGE('',*,*,#3307,.T.);
#4407=ORIENTED_EDGE('',*,*,#3308,.T.);
#4408=ORIENTED_EDGE('',*,*,#3309,.T.);
#4409=ORIENTED_EDGE('',*,*,#3268,.T.);
#4410=ORIENTED_EDGE('',*,*,#3286,.T.);
#4411=ORIENTED_EDGE('',*,*,#3304,.T.);
#4412=ORIENTED_EDGE('',*,*,#3310,.F.);
#4413=ORIENTED_EDGE('',*,*,#3296,.F.);
#4414=ORIENTED_EDGE('',*,*,#3311,.T.);
#4415=ORIENTED_EDGE('',*,*,#3290,.F.);
#4416=ORIENTED_EDGE('',*,*,#3272,.T.);
#4417=ORIENTED_EDGE('',*,*,#3306,.T.);
#4418=ORIENTED_EDGE('',*,*,#3312,.F.);
#4419=ORIENTED_EDGE('',*,*,#3297,.F.);
#4420=ORIENTED_EDGE('',*,*,#3310,.T.);
#4421=ORIENTED_EDGE('',*,*,#3305,.T.);
#4422=ORIENTED_EDGE('',*,*,#3270,.F.);
#4423=ORIENTED_EDGE('',*,*,#3292,.F.);
#4424=ORIENTED_EDGE('',*,*,#3313,.F.);
#4425=ORIENTED_EDGE('',*,*,#3298,.F.);
#4426=ORIENTED_EDGE('',*,*,#3312,.T.);
#4427=ORIENTED_EDGE('',*,*,#3301,.T.);
#4428=ORIENTED_EDGE('',*,*,#3314,.F.);
#4429=ORIENTED_EDGE('',*,*,#3315,.F.);
#4430=ORIENTED_EDGE('',*,*,#3316,.T.);
#4431=ORIENTED_EDGE('',*,*,#3302,.T.);
#4432=ORIENTED_EDGE('',*,*,#3316,.F.);
#4433=ORIENTED_EDGE('',*,*,#3317,.F.);
#4434=ORIENTED_EDGE('',*,*,#3283,.T.);
#4435=ORIENTED_EDGE('',*,*,#3303,.T.);
#4436=ORIENTED_EDGE('',*,*,#3281,.F.);
#4437=ORIENTED_EDGE('',*,*,#3318,.F.);
#4438=ORIENTED_EDGE('',*,*,#3314,.T.);
#4439=ORIENTED_EDGE('',*,*,#3315,.T.);
#4440=ORIENTED_EDGE('',*,*,#3318,.T.);
#4441=ORIENTED_EDGE('',*,*,#3280,.T.);
#4442=ORIENTED_EDGE('',*,*,#3317,.T.);
#4443=ORIENTED_EDGE('',*,*,#3307,.F.);
#4444=ORIENTED_EDGE('',*,*,#3277,.F.);
#4445=ORIENTED_EDGE('',*,*,#3319,.T.);
#4446=ORIENTED_EDGE('',*,*,#3320,.T.);
#4447=ORIENTED_EDGE('',*,*,#3308,.F.);
#4448=ORIENTED_EDGE('',*,*,#3320,.F.);
#4449=ORIENTED_EDGE('',*,*,#3321,.T.);
#4450=ORIENTED_EDGE('',*,*,#3322,.T.);
#4451=ORIENTED_EDGE('',*,*,#3309,.F.);
#4452=ORIENTED_EDGE('',*,*,#3322,.F.);
#4453=ORIENTED_EDGE('',*,*,#3323,.T.);
#4454=ORIENTED_EDGE('',*,*,#3279,.T.);
#4455=ORIENTED_EDGE('',*,*,#3276,.F.);
#4456=ORIENTED_EDGE('',*,*,#3323,.F.);
#4457=ORIENTED_EDGE('',*,*,#3321,.F.);
#4458=ORIENTED_EDGE('',*,*,#3319,.F.);
#4459=ORIENTED_EDGE('',*,*,#3294,.F.);
#4460=ORIENTED_EDGE('',*,*,#3324,.F.);
#4461=ORIENTED_EDGE('',*,*,#3325,.T.);
#4462=ORIENTED_EDGE('',*,*,#3326,.T.);
#4463=ORIENTED_EDGE('',*,*,#3293,.T.);
#4464=ORIENTED_EDGE('',*,*,#3327,.F.);
#4465=ORIENTED_EDGE('',*,*,#3328,.F.);
#4466=ORIENTED_EDGE('',*,*,#3324,.T.);
#4467=ORIENTED_EDGE('',*,*,#3300,.T.);
#4468=ORIENTED_EDGE('',*,*,#3329,.F.);
#4469=ORIENTED_EDGE('',*,*,#3330,.F.);
#4470=ORIENTED_EDGE('',*,*,#3327,.T.);
#4471=ORIENTED_EDGE('',*,*,#3329,.T.);
#4472=ORIENTED_EDGE('',*,*,#3299,.F.);
#4473=ORIENTED_EDGE('',*,*,#3313,.T.);
#4474=ORIENTED_EDGE('',*,*,#3291,.T.);
#4475=ORIENTED_EDGE('',*,*,#3311,.F.);
#4476=ORIENTED_EDGE('',*,*,#3295,.F.);
#4477=ORIENTED_EDGE('',*,*,#3326,.F.);
#4478=ORIENTED_EDGE('',*,*,#3331,.F.);
#4479=ORIENTED_EDGE('',*,*,#3325,.F.);
#4480=ORIENTED_EDGE('',*,*,#3328,.T.);
#4481=ORIENTED_EDGE('',*,*,#3330,.T.);
#4482=ORIENTED_EDGE('',*,*,#3331,.T.);
#4483=ORIENTED_EDGE('',*,*,#3287,.T.);
#4484=ORIENTED_EDGE('',*,*,#3275,.T.);
#4485=ORIENTED_EDGE('',*,*,#3284,.T.);
#4486=ORIENTED_EDGE('',*,*,#3332,.F.);
#4487=ORIENTED_EDGE('',*,*,#3333,.T.);
#4488=ORIENTED_EDGE('',*,*,#3334,.T.);
#4489=ORIENTED_EDGE('',*,*,#3335,.F.);
#4490=ORIENTED_EDGE('',*,*,#3336,.F.);
#4491=ORIENTED_EDGE('',*,*,#3337,.F.);
#4492=ORIENTED_EDGE('',*,*,#3338,.F.);
#4493=ORIENTED_EDGE('',*,*,#3339,.F.);
#4494=ORIENTED_EDGE('',*,*,#3340,.F.);
#4495=ORIENTED_EDGE('',*,*,#3341,.F.);
#4496=ORIENTED_EDGE('',*,*,#3342,.T.);
#4497=ORIENTED_EDGE('',*,*,#3339,.T.);
#4498=ORIENTED_EDGE('',*,*,#3343,.F.);
#4499=ORIENTED_EDGE('',*,*,#3344,.F.);
#4500=ORIENTED_EDGE('',*,*,#3345,.F.);
#4501=ORIENTED_EDGE('',*,*,#3346,.F.);
#4502=ORIENTED_EDGE('',*,*,#3347,.F.);
#4503=ORIENTED_EDGE('',*,*,#3348,.F.);
#4504=ORIENTED_EDGE('',*,*,#3349,.T.);
#4505=ORIENTED_EDGE('',*,*,#3346,.T.);
#4506=ORIENTED_EDGE('',*,*,#3350,.F.);
#4507=ORIENTED_EDGE('',*,*,#3351,.F.);
#4508=ORIENTED_EDGE('',*,*,#3352,.F.);
#4509=ORIENTED_EDGE('',*,*,#3353,.F.);
#4510=ORIENTED_EDGE('',*,*,#3354,.F.);
#4511=ORIENTED_EDGE('',*,*,#3351,.T.);
#4512=ORIENTED_EDGE('',*,*,#3355,.T.);
#4513=ORIENTED_EDGE('',*,*,#3356,.F.);
#4514=ORIENTED_EDGE('',*,*,#3357,.F.);
#4515=ORIENTED_EDGE('',*,*,#3358,.F.);
#4516=ORIENTED_EDGE('',*,*,#3359,.F.);
#4517=ORIENTED_EDGE('',*,*,#3360,.F.);
#4518=ORIENTED_EDGE('',*,*,#3361,.F.);
#4519=ORIENTED_EDGE('',*,*,#3358,.T.);
#4520=ORIENTED_EDGE('',*,*,#3362,.T.);
#4521=ORIENTED_EDGE('',*,*,#3363,.F.);
#4522=ORIENTED_EDGE('',*,*,#3364,.F.);
#4523=ORIENTED_EDGE('',*,*,#3365,.F.);
#4524=ORIENTED_EDGE('',*,*,#3366,.F.);
#4525=ORIENTED_EDGE('',*,*,#3367,.F.);
#4526=ORIENTED_EDGE('',*,*,#3368,.F.);
#4527=ORIENTED_EDGE('',*,*,#3369,.F.);
#4528=ORIENTED_EDGE('',*,*,#3370,.F.);
#4529=ORIENTED_EDGE('',*,*,#3371,.F.);
#4530=ORIENTED_EDGE('',*,*,#3372,.F.);
#4531=ORIENTED_EDGE('',*,*,#3373,.F.);
#4532=ORIENTED_EDGE('',*,*,#3374,.F.);
#4533=ORIENTED_EDGE('',*,*,#3375,.F.);
#4534=ORIENTED_EDGE('',*,*,#3376,.F.);
#4535=ORIENTED_EDGE('',*,*,#3377,.F.);
#4536=ORIENTED_EDGE('',*,*,#3378,.F.);
#4537=ORIENTED_EDGE('',*,*,#3379,.F.);
#4538=ORIENTED_EDGE('',*,*,#3380,.F.);
#4539=ORIENTED_EDGE('',*,*,#3381,.F.);
#4540=ORIENTED_EDGE('',*,*,#3382,.F.);
#4541=ORIENTED_EDGE('',*,*,#3383,.F.);
#4542=ORIENTED_EDGE('',*,*,#3384,.F.);
#4543=ORIENTED_EDGE('',*,*,#3385,.F.);
#4544=ORIENTED_EDGE('',*,*,#3386,.F.);
#4545=ORIENTED_EDGE('',*,*,#3387,.F.);
#4546=ORIENTED_EDGE('',*,*,#3388,.F.);
#4547=ORIENTED_EDGE('',*,*,#3389,.F.);
#4548=ORIENTED_EDGE('',*,*,#3390,.F.);
#4549=ORIENTED_EDGE('',*,*,#3391,.F.);
#4550=ORIENTED_EDGE('',*,*,#3392,.F.);
#4551=ORIENTED_EDGE('',*,*,#3393,.F.);
#4552=ORIENTED_EDGE('',*,*,#3394,.F.);
#4553=ORIENTED_EDGE('',*,*,#3395,.F.);
#4554=ORIENTED_EDGE('',*,*,#3396,.F.);
#4555=ORIENTED_EDGE('',*,*,#3397,.F.);
#4556=ORIENTED_EDGE('',*,*,#3398,.F.);
#4557=ORIENTED_EDGE('',*,*,#3399,.F.);
#4558=ORIENTED_EDGE('',*,*,#3400,.F.);
#4559=ORIENTED_EDGE('',*,*,#3401,.F.);
#4560=ORIENTED_EDGE('',*,*,#3402,.F.);
#4561=ORIENTED_EDGE('',*,*,#3403,.F.);
#4562=ORIENTED_EDGE('',*,*,#3404,.F.);
#4563=ORIENTED_EDGE('',*,*,#3405,.T.);
#4564=ORIENTED_EDGE('',*,*,#3406,.T.);
#4565=ORIENTED_EDGE('',*,*,#3407,.T.);
#4566=ORIENTED_EDGE('',*,*,#3408,.F.);
#4567=ORIENTED_EDGE('',*,*,#3409,.T.);
#4568=ORIENTED_EDGE('',*,*,#3410,.T.);
#4569=ORIENTED_EDGE('',*,*,#3411,.T.);
#4570=ORIENTED_EDGE('',*,*,#3412,.T.);
#4571=ORIENTED_EDGE('',*,*,#3413,.T.);
#4572=ORIENTED_EDGE('',*,*,#3414,.F.);
#4573=ORIENTED_EDGE('',*,*,#3415,.T.);
#4574=ORIENTED_EDGE('',*,*,#3416,.F.);
#4575=ORIENTED_EDGE('',*,*,#3417,.T.);
#4576=ORIENTED_EDGE('',*,*,#3418,.T.);
#4577=ORIENTED_EDGE('',*,*,#3419,.T.);
#4578=ORIENTED_EDGE('',*,*,#3420,.F.);
#4579=ORIENTED_EDGE('',*,*,#3421,.T.);
#4580=ORIENTED_EDGE('',*,*,#3422,.T.);
#4581=ORIENTED_EDGE('',*,*,#3423,.T.);
#4582=ORIENTED_EDGE('',*,*,#3424,.T.);
#4583=ORIENTED_EDGE('',*,*,#3425,.T.);
#4584=ORIENTED_EDGE('',*,*,#3426,.F.);
#4585=ORIENTED_EDGE('',*,*,#3427,.T.);
#4586=ORIENTED_EDGE('',*,*,#3428,.T.);
#4587=ORIENTED_EDGE('',*,*,#3429,.T.);
#4588=ORIENTED_EDGE('',*,*,#3430,.F.);
#4589=ORIENTED_EDGE('',*,*,#3431,.T.);
#4590=ORIENTED_EDGE('',*,*,#3432,.T.);
#4591=ORIENTED_EDGE('',*,*,#3433,.T.);
#4592=ORIENTED_EDGE('',*,*,#3434,.F.);
#4593=ORIENTED_EDGE('',*,*,#3435,.T.);
#4594=ORIENTED_EDGE('',*,*,#3436,.F.);
#4595=ORIENTED_EDGE('',*,*,#3437,.T.);
#4596=ORIENTED_EDGE('',*,*,#3438,.T.);
#4597=ORIENTED_EDGE('',*,*,#3439,.T.);
#4598=ORIENTED_EDGE('',*,*,#3440,.F.);
#4599=ORIENTED_EDGE('',*,*,#3441,.T.);
#4600=ORIENTED_EDGE('',*,*,#3442,.T.);
#4601=ORIENTED_EDGE('',*,*,#3443,.T.);
#4602=ORIENTED_EDGE('',*,*,#3444,.T.);
#4603=ORIENTED_EDGE('',*,*,#3445,.T.);
#4604=ORIENTED_EDGE('',*,*,#3446,.F.);
#4605=ORIENTED_EDGE('',*,*,#3447,.T.);
#4606=ORIENTED_EDGE('',*,*,#3448,.T.);
#4607=ORIENTED_EDGE('',*,*,#3449,.T.);
#4608=ORIENTED_EDGE('',*,*,#3450,.F.);
#4609=ORIENTED_EDGE('',*,*,#3451,.T.);
#4610=ORIENTED_EDGE('',*,*,#3452,.T.);
#4611=ORIENTED_EDGE('',*,*,#3453,.T.);
#4612=ORIENTED_EDGE('',*,*,#3454,.F.);
#4613=ORIENTED_EDGE('',*,*,#3455,.T.);
#4614=ORIENTED_EDGE('',*,*,#3456,.T.);
#4615=ORIENTED_EDGE('',*,*,#3457,.T.);
#4616=ORIENTED_EDGE('',*,*,#3458,.F.);
#4617=ORIENTED_EDGE('',*,*,#3459,.T.);
#4618=ORIENTED_EDGE('',*,*,#3460,.T.);
#4619=ORIENTED_EDGE('',*,*,#3461,.T.);
#4620=ORIENTED_EDGE('',*,*,#3462,.F.);
#4621=ORIENTED_EDGE('',*,*,#3341,.T.);
#4622=ORIENTED_EDGE('',*,*,#3463,.T.);
#4623=ORIENTED_EDGE('',*,*,#3464,.T.);
#4624=ORIENTED_EDGE('',*,*,#3465,.F.);
#4625=ORIENTED_EDGE('',*,*,#3348,.T.);
#4626=ORIENTED_EDGE('',*,*,#3466,.F.);
#4627=ORIENTED_EDGE('',*,*,#3467,.T.);
#4628=ORIENTED_EDGE('',*,*,#3468,.T.);
#4629=ORIENTED_EDGE('',*,*,#3363,.T.);
#4630=ORIENTED_EDGE('',*,*,#3469,.F.);
#4631=ORIENTED_EDGE('',*,*,#3470,.T.);
#4632=ORIENTED_EDGE('',*,*,#3471,.T.);
#4633=ORIENTED_EDGE('',*,*,#3472,.T.);
#4634=ORIENTED_EDGE('',*,*,#3473,.F.);
#4635=ORIENTED_EDGE('',*,*,#3474,.T.);
#4636=ORIENTED_EDGE('',*,*,#3475,.T.);
#4637=ORIENTED_EDGE('',*,*,#3476,.T.);
#4638=ORIENTED_EDGE('',*,*,#3477,.T.);
#4639=ORIENTED_EDGE('',*,*,#3478,.T.);
#4640=ORIENTED_EDGE('',*,*,#3479,.F.);
#4641=ORIENTED_EDGE('',*,*,#3480,.T.);
#4642=ORIENTED_EDGE('',*,*,#3481,.F.);
#4643=ORIENTED_EDGE('',*,*,#3482,.T.);
#4644=ORIENTED_EDGE('',*,*,#3483,.T.);
#4645=ORIENTED_EDGE('',*,*,#3484,.T.);
#4646=ORIENTED_EDGE('',*,*,#3485,.F.);
#4647=ORIENTED_EDGE('',*,*,#3486,.T.);
#4648=ORIENTED_EDGE('',*,*,#3487,.T.);
#4649=ORIENTED_EDGE('',*,*,#3488,.T.);
#4650=ORIENTED_EDGE('',*,*,#3489,.F.);
#4651=ORIENTED_EDGE('',*,*,#3490,.T.);
#4652=ORIENTED_EDGE('',*,*,#3491,.T.);
#4653=ORIENTED_EDGE('',*,*,#3492,.T.);
#4654=ORIENTED_EDGE('',*,*,#3493,.F.);
#4655=ORIENTED_EDGE('',*,*,#3494,.T.);
#4656=ORIENTED_EDGE('',*,*,#3495,.T.);
#4657=ORIENTED_EDGE('',*,*,#3496,.T.);
#4658=ORIENTED_EDGE('',*,*,#3497,.F.);
#4659=ORIENTED_EDGE('',*,*,#3498,.T.);
#4660=ORIENTED_EDGE('',*,*,#3499,.T.);
#4661=ORIENTED_EDGE('',*,*,#3500,.T.);
#4662=ORIENTED_EDGE('',*,*,#3501,.T.);
#4663=ORIENTED_EDGE('',*,*,#3502,.T.);
#4664=ORIENTED_EDGE('',*,*,#3503,.F.);
#4665=ORIENTED_EDGE('',*,*,#3504,.T.);
#4666=ORIENTED_EDGE('',*,*,#3505,.T.);
#4667=ORIENTED_EDGE('',*,*,#3506,.T.);
#4668=ORIENTED_EDGE('',*,*,#3507,.F.);
#4669=ORIENTED_EDGE('',*,*,#3508,.T.);
#4670=ORIENTED_EDGE('',*,*,#3509,.T.);
#4671=ORIENTED_EDGE('',*,*,#3510,.T.);
#4672=ORIENTED_EDGE('',*,*,#3511,.F.);
#4673=ORIENTED_EDGE('',*,*,#3512,.T.);
#4674=ORIENTED_EDGE('',*,*,#3513,.F.);
#4675=ORIENTED_EDGE('',*,*,#3514,.T.);
#4676=ORIENTED_EDGE('',*,*,#3515,.T.);
#4677=ORIENTED_EDGE('',*,*,#3516,.T.);
#4678=ORIENTED_EDGE('',*,*,#3410,.F.);
#4679=ORIENTED_EDGE('',*,*,#3517,.T.);
#4680=ORIENTED_EDGE('',*,*,#3518,.T.);
#4681=ORIENTED_EDGE('',*,*,#3519,.T.);
#4682=ORIENTED_EDGE('',*,*,#3520,.T.);
#4683=ORIENTED_EDGE('',*,*,#3521,.T.);
#4684=ORIENTED_EDGE('',*,*,#3412,.F.);
#4685=ORIENTED_EDGE('',*,*,#3522,.T.);
#4686=ORIENTED_EDGE('',*,*,#3523,.T.);
#4687=ORIENTED_EDGE('',*,*,#3524,.T.);
#4688=ORIENTED_EDGE('',*,*,#3525,.T.);
#4689=ORIENTED_EDGE('',*,*,#3526,.T.);
#4690=ORIENTED_EDGE('',*,*,#3424,.F.);
#4691=ORIENTED_EDGE('',*,*,#3527,.T.);
#4692=ORIENTED_EDGE('',*,*,#3528,.T.);
#4693=ORIENTED_EDGE('',*,*,#3529,.T.);
#4694=ORIENTED_EDGE('',*,*,#3530,.T.);
#4695=ORIENTED_EDGE('',*,*,#3531,.T.);
#4696=ORIENTED_EDGE('',*,*,#3428,.F.);
#4697=ORIENTED_EDGE('',*,*,#3532,.T.);
#4698=ORIENTED_EDGE('',*,*,#3533,.T.);
#4699=ORIENTED_EDGE('',*,*,#3534,.T.);
#4700=ORIENTED_EDGE('',*,*,#3535,.T.);
#4701=ORIENTED_EDGE('',*,*,#3536,.T.);
#4702=ORIENTED_EDGE('',*,*,#3406,.F.);
#4703=ORIENTED_EDGE('',*,*,#3537,.T.);
#4704=ORIENTED_EDGE('',*,*,#3538,.T.);
#4705=ORIENTED_EDGE('',*,*,#3539,.T.);
#4706=ORIENTED_EDGE('',*,*,#3540,.T.);
#4707=ORIENTED_EDGE('',*,*,#3541,.T.);
#4708=ORIENTED_EDGE('',*,*,#3432,.F.);
#4709=ORIENTED_EDGE('',*,*,#3542,.T.);
#4710=ORIENTED_EDGE('',*,*,#3543,.T.);
#4711=ORIENTED_EDGE('',*,*,#3544,.T.);
#4712=ORIENTED_EDGE('',*,*,#3545,.T.);
#4713=ORIENTED_EDGE('',*,*,#3546,.T.);
#4714=ORIENTED_EDGE('',*,*,#3444,.F.);
#4715=ORIENTED_EDGE('',*,*,#3547,.T.);
#4716=ORIENTED_EDGE('',*,*,#3548,.T.);
#4717=ORIENTED_EDGE('',*,*,#3549,.T.);
#4718=ORIENTED_EDGE('',*,*,#3550,.T.);
#4719=ORIENTED_EDGE('',*,*,#3551,.T.);
#4720=ORIENTED_EDGE('',*,*,#3448,.F.);
#4721=ORIENTED_EDGE('',*,*,#3552,.T.);
#4722=ORIENTED_EDGE('',*,*,#3553,.T.);
#4723=ORIENTED_EDGE('',*,*,#3554,.T.);
#4724=ORIENTED_EDGE('',*,*,#3555,.T.);
#4725=ORIENTED_EDGE('',*,*,#3556,.T.);
#4726=ORIENTED_EDGE('',*,*,#3442,.F.);
#4727=ORIENTED_EDGE('',*,*,#3557,.T.);
#4728=ORIENTED_EDGE('',*,*,#3558,.T.);
#4729=ORIENTED_EDGE('',*,*,#3559,.T.);
#4730=ORIENTED_EDGE('',*,*,#3560,.T.);
#4731=ORIENTED_EDGE('',*,*,#3561,.T.);
#4732=ORIENTED_EDGE('',*,*,#3438,.F.);
#4733=ORIENTED_EDGE('',*,*,#3562,.T.);
#4734=ORIENTED_EDGE('',*,*,#3563,.T.);
#4735=ORIENTED_EDGE('',*,*,#3564,.T.);
#4736=ORIENTED_EDGE('',*,*,#3565,.T.);
#4737=ORIENTED_EDGE('',*,*,#3566,.T.);
#4738=ORIENTED_EDGE('',*,*,#3452,.F.);
#4739=ORIENTED_EDGE('',*,*,#3567,.T.);
#4740=ORIENTED_EDGE('',*,*,#3568,.T.);
#4741=ORIENTED_EDGE('',*,*,#3569,.T.);
#4742=ORIENTED_EDGE('',*,*,#3570,.T.);
#4743=ORIENTED_EDGE('',*,*,#3571,.T.);
#4744=ORIENTED_EDGE('',*,*,#3456,.F.);
#4745=ORIENTED_EDGE('',*,*,#3572,.T.);
#4746=ORIENTED_EDGE('',*,*,#3573,.T.);
#4747=ORIENTED_EDGE('',*,*,#3574,.T.);
#4748=ORIENTED_EDGE('',*,*,#3575,.T.);
#4749=ORIENTED_EDGE('',*,*,#3576,.T.);
#4750=ORIENTED_EDGE('',*,*,#3460,.F.);
#4751=ORIENTED_EDGE('',*,*,#3340,.T.);
#4752=ORIENTED_EDGE('',*,*,#3338,.T.);
#4753=ORIENTED_EDGE('',*,*,#3577,.T.);
#4754=ORIENTED_EDGE('',*,*,#3578,.T.);
#4755=ORIENTED_EDGE('',*,*,#3579,.T.);
#4756=ORIENTED_EDGE('',*,*,#3463,.F.);
#4757=ORIENTED_EDGE('',*,*,#3347,.T.);
#4758=ORIENTED_EDGE('',*,*,#3345,.T.);
#4759=ORIENTED_EDGE('',*,*,#3580,.T.);
#4760=ORIENTED_EDGE('',*,*,#3581,.T.);
#4761=ORIENTED_EDGE('',*,*,#3582,.T.);
#4762=ORIENTED_EDGE('',*,*,#3501,.F.);
#4763=ORIENTED_EDGE('',*,*,#3583,.T.);
#4764=ORIENTED_EDGE('',*,*,#3394,.T.);
#4765=ORIENTED_EDGE('',*,*,#3584,.T.);
#4766=ORIENTED_EDGE('',*,*,#3585,.T.);
#4767=ORIENTED_EDGE('',*,*,#3586,.T.);
#4768=ORIENTED_EDGE('',*,*,#3499,.F.);
#4769=ORIENTED_EDGE('',*,*,#3587,.T.);
#4770=ORIENTED_EDGE('',*,*,#3390,.T.);
#4771=ORIENTED_EDGE('',*,*,#3588,.T.);
#4772=ORIENTED_EDGE('',*,*,#3589,.T.);
#4773=ORIENTED_EDGE('',*,*,#3590,.T.);
#4774=ORIENTED_EDGE('',*,*,#3505,.F.);
#4775=ORIENTED_EDGE('',*,*,#3591,.T.);
#4776=ORIENTED_EDGE('',*,*,#3398,.T.);
#4777=ORIENTED_EDGE('',*,*,#3592,.T.);
#4778=ORIENTED_EDGE('',*,*,#3593,.T.);
#4779=ORIENTED_EDGE('',*,*,#3594,.T.);
#4780=ORIENTED_EDGE('',*,*,#3509,.F.);
#4781=ORIENTED_EDGE('',*,*,#3595,.T.);
#4782=ORIENTED_EDGE('',*,*,#3402,.T.);
#4783=ORIENTED_EDGE('',*,*,#3596,.T.);
#4784=ORIENTED_EDGE('',*,*,#3597,.T.);
#4785=ORIENTED_EDGE('',*,*,#3598,.T.);
#4786=ORIENTED_EDGE('',*,*,#3495,.F.);
#4787=ORIENTED_EDGE('',*,*,#3599,.T.);
#4788=ORIENTED_EDGE('',*,*,#3386,.T.);
#4789=ORIENTED_EDGE('',*,*,#3600,.T.);
#4790=ORIENTED_EDGE('',*,*,#3601,.T.);
#4791=ORIENTED_EDGE('',*,*,#3602,.T.);
#4792=ORIENTED_EDGE('',*,*,#3491,.F.);
#4793=ORIENTED_EDGE('',*,*,#3603,.T.);
#4794=ORIENTED_EDGE('',*,*,#3604,.T.);
#4795=ORIENTED_EDGE('',*,*,#3605,.T.);
#4796=ORIENTED_EDGE('',*,*,#3382,.T.);
#4797=ORIENTED_EDGE('',*,*,#3606,.T.);
#4798=ORIENTED_EDGE('',*,*,#3487,.F.);
#4799=ORIENTED_EDGE('',*,*,#3607,.T.);
#4800=ORIENTED_EDGE('',*,*,#3608,.T.);
#4801=ORIENTED_EDGE('',*,*,#3609,.T.);
#4802=ORIENTED_EDGE('',*,*,#3378,.T.);
#4803=ORIENTED_EDGE('',*,*,#3610,.T.);
#4804=ORIENTED_EDGE('',*,*,#3483,.F.);
#4805=ORIENTED_EDGE('',*,*,#3611,.T.);
#4806=ORIENTED_EDGE('',*,*,#3612,.T.);
#4807=ORIENTED_EDGE('',*,*,#3613,.T.);
#4808=ORIENTED_EDGE('',*,*,#3374,.T.);
#4809=ORIENTED_EDGE('',*,*,#3614,.T.);
#4810=ORIENTED_EDGE('',*,*,#3475,.F.);
#4811=ORIENTED_EDGE('',*,*,#3615,.T.);
#4812=ORIENTED_EDGE('',*,*,#3616,.T.);
#4813=ORIENTED_EDGE('',*,*,#3617,.T.);
#4814=ORIENTED_EDGE('',*,*,#3366,.T.);
#4815=ORIENTED_EDGE('',*,*,#3618,.T.);
#4816=ORIENTED_EDGE('',*,*,#3477,.F.);
#4817=ORIENTED_EDGE('',*,*,#3619,.T.);
#4818=ORIENTED_EDGE('',*,*,#3620,.T.);
#4819=ORIENTED_EDGE('',*,*,#3621,.T.);
#4820=ORIENTED_EDGE('',*,*,#3370,.T.);
#4821=ORIENTED_EDGE('',*,*,#3622,.T.);
#4822=ORIENTED_EDGE('',*,*,#3471,.F.);
#4823=ORIENTED_EDGE('',*,*,#3623,.T.);
#4824=ORIENTED_EDGE('',*,*,#3624,.T.);
#4825=ORIENTED_EDGE('',*,*,#3625,.T.);
#4826=ORIENTED_EDGE('',*,*,#3359,.T.);
#4827=ORIENTED_EDGE('',*,*,#3361,.T.);
#4828=ORIENTED_EDGE('',*,*,#3468,.F.);
#4829=ORIENTED_EDGE('',*,*,#3626,.T.);
#4830=ORIENTED_EDGE('',*,*,#3627,.T.);
#4831=ORIENTED_EDGE('',*,*,#3628,.T.);
#4832=ORIENTED_EDGE('',*,*,#3352,.T.);
#4833=ORIENTED_EDGE('',*,*,#3354,.T.);
#4834=ORIENTED_EDGE('',*,*,#3629,.F.);
#4835=ORIENTED_EDGE('',*,*,#3630,.T.);
#4836=ORIENTED_EDGE('',*,*,#3631,.T.);
#4837=ORIENTED_EDGE('',*,*,#3632,.T.);
#4838=ORIENTED_EDGE('',*,*,#3633,.T.);
#4839=ORIENTED_EDGE('',*,*,#3634,.T.);
#4840=ORIENTED_EDGE('',*,*,#3515,.F.);
#4841=ORIENTED_EDGE('',*,*,#3635,.T.);
#4842=ORIENTED_EDGE('',*,*,#3636,.T.);
#4843=ORIENTED_EDGE('',*,*,#3637,.T.);
#4844=ORIENTED_EDGE('',*,*,#3638,.T.);
#4845=ORIENTED_EDGE('',*,*,#3639,.T.);
#4846=ORIENTED_EDGE('',*,*,#3422,.F.);
#4847=ORIENTED_EDGE('',*,*,#3640,.T.);
#4848=ORIENTED_EDGE('',*,*,#3641,.T.);
#4849=ORIENTED_EDGE('',*,*,#3642,.T.);
#4850=ORIENTED_EDGE('',*,*,#3643,.T.);
#4851=ORIENTED_EDGE('',*,*,#3644,.T.);
#4852=ORIENTED_EDGE('',*,*,#3418,.F.);
#4853=ORIENTED_EDGE('',*,*,#3645,.T.);
#4854=ORIENTED_EDGE('',*,*,#3646,.T.);
#4855=ORIENTED_EDGE('',*,*,#3647,.T.);
#4856=ORIENTED_EDGE('',*,*,#3648,.T.);
#4857=ORIENTED_EDGE('',*,*,#3649,.T.);
#4858=ORIENTED_EDGE('',*,*,#3650,.T.);
#4859=ORIENTED_EDGE('',*,*,#3332,.T.);
#4860=ORIENTED_EDGE('',*,*,#3651,.T.);
#4861=ORIENTED_EDGE('',*,*,#3652,.T.);
#4862=ORIENTED_EDGE('',*,*,#3653,.F.);
#4863=ORIENTED_EDGE('',*,*,#3408,.T.);
#4864=ORIENTED_EDGE('',*,*,#3654,.F.);
#4865=ORIENTED_EDGE('',*,*,#3655,.T.);
#4866=ORIENTED_EDGE('',*,*,#3656,.F.);
#4867=ORIENTED_EDGE('',*,*,#3657,.T.);
#4868=ORIENTED_EDGE('',*,*,#3658,.F.);
#4869=ORIENTED_EDGE('',*,*,#3416,.T.);
#4870=ORIENTED_EDGE('',*,*,#3659,.F.);
#4871=ORIENTED_EDGE('',*,*,#3660,.T.);
#4872=ORIENTED_EDGE('',*,*,#3661,.F.);
#4873=ORIENTED_EDGE('',*,*,#3662,.T.);
#4874=ORIENTED_EDGE('',*,*,#3663,.F.);
#4875=ORIENTED_EDGE('',*,*,#3420,.T.);
#4876=ORIENTED_EDGE('',*,*,#3664,.F.);
#4877=ORIENTED_EDGE('',*,*,#3665,.T.);
#4878=ORIENTED_EDGE('',*,*,#3666,.F.);
#4879=ORIENTED_EDGE('',*,*,#3667,.T.);
#4880=ORIENTED_EDGE('',*,*,#3668,.F.);
#4881=ORIENTED_EDGE('',*,*,#3513,.T.);
#4882=ORIENTED_EDGE('',*,*,#3669,.F.);
#4883=ORIENTED_EDGE('',*,*,#3670,.T.);
#4884=ORIENTED_EDGE('',*,*,#3671,.F.);
#4885=ORIENTED_EDGE('',*,*,#3672,.T.);
#4886=ORIENTED_EDGE('',*,*,#3673,.F.);
#4887=ORIENTED_EDGE('',*,*,#3674,.T.);
#4888=ORIENTED_EDGE('',*,*,#3355,.F.);
#4889=ORIENTED_EDGE('',*,*,#3350,.T.);
#4890=ORIENTED_EDGE('',*,*,#3675,.F.);
#4891=ORIENTED_EDGE('',*,*,#3676,.T.);
#4892=ORIENTED_EDGE('',*,*,#3677,.F.);
#4893=ORIENTED_EDGE('',*,*,#3466,.T.);
#4894=ORIENTED_EDGE('',*,*,#3362,.F.);
#4895=ORIENTED_EDGE('',*,*,#3357,.T.);
#4896=ORIENTED_EDGE('',*,*,#3678,.F.);
#4897=ORIENTED_EDGE('',*,*,#3679,.T.);
#4898=ORIENTED_EDGE('',*,*,#3680,.F.);
#4899=ORIENTED_EDGE('',*,*,#3469,.T.);
#4900=ORIENTED_EDGE('',*,*,#3681,.F.);
#4901=ORIENTED_EDGE('',*,*,#3368,.T.);
#4902=ORIENTED_EDGE('',*,*,#3682,.F.);
#4903=ORIENTED_EDGE('',*,*,#3683,.T.);
#4904=ORIENTED_EDGE('',*,*,#3684,.F.);
#4905=ORIENTED_EDGE('',*,*,#3479,.T.);
#4906=ORIENTED_EDGE('',*,*,#3685,.F.);
#4907=ORIENTED_EDGE('',*,*,#3364,.T.);
#4908=ORIENTED_EDGE('',*,*,#3686,.F.);
#4909=ORIENTED_EDGE('',*,*,#3687,.T.);
#4910=ORIENTED_EDGE('',*,*,#3688,.F.);
#4911=ORIENTED_EDGE('',*,*,#3473,.T.);
#4912=ORIENTED_EDGE('',*,*,#3689,.F.);
#4913=ORIENTED_EDGE('',*,*,#3372,.T.);
#4914=ORIENTED_EDGE('',*,*,#3690,.F.);
#4915=ORIENTED_EDGE('',*,*,#3691,.T.);
#4916=ORIENTED_EDGE('',*,*,#3692,.F.);
#4917=ORIENTED_EDGE('',*,*,#3481,.T.);
#4918=ORIENTED_EDGE('',*,*,#3693,.F.);
#4919=ORIENTED_EDGE('',*,*,#3376,.T.);
#4920=ORIENTED_EDGE('',*,*,#3694,.F.);
#4921=ORIENTED_EDGE('',*,*,#3695,.T.);
#4922=ORIENTED_EDGE('',*,*,#3696,.F.);
#4923=ORIENTED_EDGE('',*,*,#3485,.T.);
#4924=ORIENTED_EDGE('',*,*,#3697,.F.);
#4925=ORIENTED_EDGE('',*,*,#3380,.T.);
#4926=ORIENTED_EDGE('',*,*,#3698,.F.);
#4927=ORIENTED_EDGE('',*,*,#3699,.T.);
#4928=ORIENTED_EDGE('',*,*,#3700,.F.);
#4929=ORIENTED_EDGE('',*,*,#3489,.T.);
#4930=ORIENTED_EDGE('',*,*,#3701,.F.);
#4931=ORIENTED_EDGE('',*,*,#3702,.T.);
#4932=ORIENTED_EDGE('',*,*,#3703,.F.);
#4933=ORIENTED_EDGE('',*,*,#3384,.T.);
#4934=ORIENTED_EDGE('',*,*,#3704,.F.);
#4935=ORIENTED_EDGE('',*,*,#3493,.T.);
#4936=ORIENTED_EDGE('',*,*,#3705,.F.);
#4937=ORIENTED_EDGE('',*,*,#3706,.T.);
#4938=ORIENTED_EDGE('',*,*,#3707,.F.);
#4939=ORIENTED_EDGE('',*,*,#3400,.T.);
#4940=ORIENTED_EDGE('',*,*,#3708,.F.);
#4941=ORIENTED_EDGE('',*,*,#3511,.T.);
#4942=ORIENTED_EDGE('',*,*,#3709,.F.);
#4943=ORIENTED_EDGE('',*,*,#3710,.T.);
#4944=ORIENTED_EDGE('',*,*,#3711,.F.);
#4945=ORIENTED_EDGE('',*,*,#3396,.T.);
#4946=ORIENTED_EDGE('',*,*,#3712,.F.);
#4947=ORIENTED_EDGE('',*,*,#3507,.T.);
#4948=ORIENTED_EDGE('',*,*,#3713,.F.);
#4949=ORIENTED_EDGE('',*,*,#3714,.T.);
#4950=ORIENTED_EDGE('',*,*,#3715,.F.);
#4951=ORIENTED_EDGE('',*,*,#3388,.T.);
#4952=ORIENTED_EDGE('',*,*,#3716,.F.);
#4953=ORIENTED_EDGE('',*,*,#3497,.T.);
#4954=ORIENTED_EDGE('',*,*,#3717,.F.);
#4955=ORIENTED_EDGE('',*,*,#3718,.T.);
#4956=ORIENTED_EDGE('',*,*,#3719,.F.);
#4957=ORIENTED_EDGE('',*,*,#3392,.T.);
#4958=ORIENTED_EDGE('',*,*,#3720,.F.);
#4959=ORIENTED_EDGE('',*,*,#3503,.T.);
#4960=ORIENTED_EDGE('',*,*,#3721,.F.);
#4961=ORIENTED_EDGE('',*,*,#3722,.T.);
#4962=ORIENTED_EDGE('',*,*,#3723,.F.);
#4963=ORIENTED_EDGE('',*,*,#3343,.T.);
#4964=ORIENTED_EDGE('',*,*,#3349,.F.);
#4965=ORIENTED_EDGE('',*,*,#3465,.T.);
#4966=ORIENTED_EDGE('',*,*,#3724,.F.);
#4967=ORIENTED_EDGE('',*,*,#3725,.T.);
#4968=ORIENTED_EDGE('',*,*,#3726,.F.);
#4969=ORIENTED_EDGE('',*,*,#3336,.T.);
#4970=ORIENTED_EDGE('',*,*,#3342,.F.);
#4971=ORIENTED_EDGE('',*,*,#3462,.T.);
#4972=ORIENTED_EDGE('',*,*,#3727,.F.);
#4973=ORIENTED_EDGE('',*,*,#3728,.T.);
#4974=ORIENTED_EDGE('',*,*,#3729,.F.);
#4975=ORIENTED_EDGE('',*,*,#3730,.T.);
#4976=ORIENTED_EDGE('',*,*,#3731,.F.);
#4977=ORIENTED_EDGE('',*,*,#3458,.T.);
#4978=ORIENTED_EDGE('',*,*,#3732,.F.);
#4979=ORIENTED_EDGE('',*,*,#3733,.T.);
#4980=ORIENTED_EDGE('',*,*,#3734,.F.);
#4981=ORIENTED_EDGE('',*,*,#3735,.T.);
#4982=ORIENTED_EDGE('',*,*,#3736,.F.);
#4983=ORIENTED_EDGE('',*,*,#3454,.T.);
#4984=ORIENTED_EDGE('',*,*,#3737,.F.);
#4985=ORIENTED_EDGE('',*,*,#3738,.T.);
#4986=ORIENTED_EDGE('',*,*,#3739,.F.);
#4987=ORIENTED_EDGE('',*,*,#3740,.T.);
#4988=ORIENTED_EDGE('',*,*,#3741,.F.);
#4989=ORIENTED_EDGE('',*,*,#3436,.T.);
#4990=ORIENTED_EDGE('',*,*,#3742,.F.);
#4991=ORIENTED_EDGE('',*,*,#3743,.T.);
#4992=ORIENTED_EDGE('',*,*,#3744,.F.);
#4993=ORIENTED_EDGE('',*,*,#3745,.T.);
#4994=ORIENTED_EDGE('',*,*,#3746,.F.);
#4995=ORIENTED_EDGE('',*,*,#3440,.T.);
#4996=ORIENTED_EDGE('',*,*,#3747,.F.);
#4997=ORIENTED_EDGE('',*,*,#3748,.T.);
#4998=ORIENTED_EDGE('',*,*,#3749,.F.);
#4999=ORIENTED_EDGE('',*,*,#3750,.T.);
#5000=ORIENTED_EDGE('',*,*,#3751,.F.);
#5001=ORIENTED_EDGE('',*,*,#3450,.T.);
#5002=ORIENTED_EDGE('',*,*,#3752,.F.);
#5003=ORIENTED_EDGE('',*,*,#3753,.T.);
#5004=ORIENTED_EDGE('',*,*,#3754,.F.);
#5005=ORIENTED_EDGE('',*,*,#3755,.T.);
#5006=ORIENTED_EDGE('',*,*,#3756,.F.);
#5007=ORIENTED_EDGE('',*,*,#3446,.T.);
#5008=ORIENTED_EDGE('',*,*,#3757,.F.);
#5009=ORIENTED_EDGE('',*,*,#3758,.T.);
#5010=ORIENTED_EDGE('',*,*,#3759,.F.);
#5011=ORIENTED_EDGE('',*,*,#3760,.T.);
#5012=ORIENTED_EDGE('',*,*,#3761,.F.);
#5013=ORIENTED_EDGE('',*,*,#3434,.T.);
#5014=ORIENTED_EDGE('',*,*,#3762,.F.);
#5015=ORIENTED_EDGE('',*,*,#3763,.T.);
#5016=ORIENTED_EDGE('',*,*,#3764,.F.);
#5017=ORIENTED_EDGE('',*,*,#3765,.T.);
#5018=ORIENTED_EDGE('',*,*,#3766,.F.);
#5019=ORIENTED_EDGE('',*,*,#3404,.T.);
#5020=ORIENTED_EDGE('',*,*,#3767,.F.);
#5021=ORIENTED_EDGE('',*,*,#3768,.T.);
#5022=ORIENTED_EDGE('',*,*,#3769,.F.);
#5023=ORIENTED_EDGE('',*,*,#3770,.T.);
#5024=ORIENTED_EDGE('',*,*,#3771,.F.);
#5025=ORIENTED_EDGE('',*,*,#3430,.T.);
#5026=ORIENTED_EDGE('',*,*,#3772,.F.);
#5027=ORIENTED_EDGE('',*,*,#3773,.T.);
#5028=ORIENTED_EDGE('',*,*,#3774,.F.);
#5029=ORIENTED_EDGE('',*,*,#3775,.T.);
#5030=ORIENTED_EDGE('',*,*,#3776,.F.);
#5031=ORIENTED_EDGE('',*,*,#3426,.T.);
#5032=ORIENTED_EDGE('',*,*,#3777,.F.);
#5033=ORIENTED_EDGE('',*,*,#3778,.T.);
#5034=ORIENTED_EDGE('',*,*,#3779,.F.);
#5035=ORIENTED_EDGE('',*,*,#3780,.T.);
#5036=ORIENTED_EDGE('',*,*,#3781,.F.);
#5037=ORIENTED_EDGE('',*,*,#3414,.T.);
#5038=ORIENTED_EDGE('',*,*,#3782,.F.);
#5039=ORIENTED_EDGE('',*,*,#3783,.T.);
#5040=ORIENTED_EDGE('',*,*,#3784,.F.);
#5041=ORIENTED_EDGE('',*,*,#3785,.T.);
#5042=ORIENTED_EDGE('',*,*,#3334,.F.);
#5043=ORIENTED_EDGE('',*,*,#3786,.F.);
#5044=ORIENTED_EDGE('',*,*,#3787,.F.);
#5045=ORIENTED_EDGE('',*,*,#3788,.F.);
#5046=ORIENTED_EDGE('',*,*,#3629,.T.);
#5047=ORIENTED_EDGE('',*,*,#3356,.T.);
#5048=ORIENTED_EDGE('',*,*,#3674,.F.);
#5049=ORIENTED_EDGE('',*,*,#3789,.T.);
#5050=ORIENTED_EDGE('',*,*,#3634,.F.);
#5051=ORIENTED_EDGE('',*,*,#3790,.T.);
#5052=ORIENTED_EDGE('',*,*,#3669,.T.);
#5053=ORIENTED_EDGE('',*,*,#3516,.F.);
#5054=ORIENTED_EDGE('',*,*,#3673,.T.);
#5055=ORIENTED_EDGE('',*,*,#3791,.T.);
#5056=ORIENTED_EDGE('',*,*,#3630,.F.);
#5057=ORIENTED_EDGE('',*,*,#3789,.F.);
#5058=ORIENTED_EDGE('',*,*,#3671,.T.);
#5059=ORIENTED_EDGE('',*,*,#3792,.T.);
#5060=ORIENTED_EDGE('',*,*,#3632,.F.);
#5061=ORIENTED_EDGE('',*,*,#3793,.T.);
#5062=ORIENTED_EDGE('',*,*,#3633,.F.);
#5063=ORIENTED_EDGE('',*,*,#3792,.F.);
#5064=ORIENTED_EDGE('',*,*,#3670,.F.);
#5065=ORIENTED_EDGE('',*,*,#3790,.F.);
#5066=ORIENTED_EDGE('',*,*,#3631,.F.);
#5067=ORIENTED_EDGE('',*,*,#3791,.F.);
#5068=ORIENTED_EDGE('',*,*,#3672,.F.);
#5069=ORIENTED_EDGE('',*,*,#3793,.F.);
#5070=ORIENTED_EDGE('',*,*,#3668,.T.);
#5071=ORIENTED_EDGE('',*,*,#3794,.T.);
#5072=ORIENTED_EDGE('',*,*,#3635,.F.);
#5073=ORIENTED_EDGE('',*,*,#3514,.F.);
#5074=ORIENTED_EDGE('',*,*,#3639,.F.);
#5075=ORIENTED_EDGE('',*,*,#3795,.T.);
#5076=ORIENTED_EDGE('',*,*,#3664,.T.);
#5077=ORIENTED_EDGE('',*,*,#3423,.F.);
#5078=ORIENTED_EDGE('',*,*,#3638,.F.);
#5079=ORIENTED_EDGE('',*,*,#3796,.F.);
#5080=ORIENTED_EDGE('',*,*,#3665,.F.);
#5081=ORIENTED_EDGE('',*,*,#3795,.F.);
#5082=ORIENTED_EDGE('',*,*,#3666,.T.);
#5083=ORIENTED_EDGE('',*,*,#3796,.T.);
#5084=ORIENTED_EDGE('',*,*,#3637,.F.);
#5085=ORIENTED_EDGE('',*,*,#3797,.T.);
#5086=ORIENTED_EDGE('',*,*,#3636,.F.);
#5087=ORIENTED_EDGE('',*,*,#3794,.F.);
#5088=ORIENTED_EDGE('',*,*,#3667,.F.);
#5089=ORIENTED_EDGE('',*,*,#3797,.F.);
#5090=ORIENTED_EDGE('',*,*,#3708,.T.);
#5091=ORIENTED_EDGE('',*,*,#3403,.T.);
#5092=ORIENTED_EDGE('',*,*,#3595,.F.);
#5093=ORIENTED_EDGE('',*,*,#3512,.F.);
#5094=ORIENTED_EDGE('',*,*,#3598,.F.);
#5095=ORIENTED_EDGE('',*,*,#3798,.T.);
#5096=ORIENTED_EDGE('',*,*,#3705,.T.);
#5097=ORIENTED_EDGE('',*,*,#3496,.F.);
#5098=ORIENTED_EDGE('',*,*,#3597,.F.);
#5099=ORIENTED_EDGE('',*,*,#3799,.F.);
#5100=ORIENTED_EDGE('',*,*,#3706,.F.);
#5101=ORIENTED_EDGE('',*,*,#3798,.F.);
#5102=ORIENTED_EDGE('',*,*,#3707,.T.);
#5103=ORIENTED_EDGE('',*,*,#3799,.T.);
#5104=ORIENTED_EDGE('',*,*,#3596,.F.);
#5105=ORIENTED_EDGE('',*,*,#3401,.T.);
#5106=ORIENTED_EDGE('',*,*,#3712,.T.);
#5107=ORIENTED_EDGE('',*,*,#3399,.T.);
#5108=ORIENTED_EDGE('',*,*,#3591,.F.);
#5109=ORIENTED_EDGE('',*,*,#3508,.F.);
#5110=ORIENTED_EDGE('',*,*,#3594,.F.);
#5111=ORIENTED_EDGE('',*,*,#3800,.T.);
#5112=ORIENTED_EDGE('',*,*,#3709,.T.);
#5113=ORIENTED_EDGE('',*,*,#3510,.F.);
#5114=ORIENTED_EDGE('',*,*,#3593,.F.);
#5115=ORIENTED_EDGE('',*,*,#3801,.F.);
#5116=ORIENTED_EDGE('',*,*,#3710,.F.);
#5117=ORIENTED_EDGE('',*,*,#3800,.F.);
#5118=ORIENTED_EDGE('',*,*,#3711,.T.);
#5119=ORIENTED_EDGE('',*,*,#3801,.T.);
#5120=ORIENTED_EDGE('',*,*,#3592,.F.);
#5121=ORIENTED_EDGE('',*,*,#3397,.T.);
#5122=ORIENTED_EDGE('',*,*,#3720,.T.);
#5123=ORIENTED_EDGE('',*,*,#3395,.T.);
#5124=ORIENTED_EDGE('',*,*,#3583,.F.);
#5125=ORIENTED_EDGE('',*,*,#3504,.F.);
#5126=ORIENTED_EDGE('',*,*,#3586,.F.);
#5127=ORIENTED_EDGE('',*,*,#3802,.T.);
#5128=ORIENTED_EDGE('',*,*,#3717,.T.);
#5129=ORIENTED_EDGE('',*,*,#3500,.F.);
#5130=ORIENTED_EDGE('',*,*,#3585,.F.);
#5131=ORIENTED_EDGE('',*,*,#3803,.F.);
#5132=ORIENTED_EDGE('',*,*,#3718,.F.);
#5133=ORIENTED_EDGE('',*,*,#3802,.F.);
#5134=ORIENTED_EDGE('',*,*,#3719,.T.);
#5135=ORIENTED_EDGE('',*,*,#3803,.T.);
#5136=ORIENTED_EDGE('',*,*,#3584,.F.);
#5137=ORIENTED_EDGE('',*,*,#3393,.T.);
#5138=ORIENTED_EDGE('',*,*,#3716,.T.);
#5139=ORIENTED_EDGE('',*,*,#3391,.T.);
#5140=ORIENTED_EDGE('',*,*,#3587,.F.);
#5141=ORIENTED_EDGE('',*,*,#3498,.F.);
#5142=ORIENTED_EDGE('',*,*,#3590,.F.);
#5143=ORIENTED_EDGE('',*,*,#3804,.T.);
#5144=ORIENTED_EDGE('',*,*,#3713,.T.);
#5145=ORIENTED_EDGE('',*,*,#3506,.F.);
#5146=ORIENTED_EDGE('',*,*,#3589,.F.);
#5147=ORIENTED_EDGE('',*,*,#3805,.F.);
#5148=ORIENTED_EDGE('',*,*,#3714,.F.);
#5149=ORIENTED_EDGE('',*,*,#3804,.F.);
#5150=ORIENTED_EDGE('',*,*,#3715,.T.);
#5151=ORIENTED_EDGE('',*,*,#3805,.T.);
#5152=ORIENTED_EDGE('',*,*,#3588,.F.);
#5153=ORIENTED_EDGE('',*,*,#3389,.T.);
#5154=ORIENTED_EDGE('',*,*,#3704,.T.);
#5155=ORIENTED_EDGE('',*,*,#3387,.T.);
#5156=ORIENTED_EDGE('',*,*,#3599,.F.);
#5157=ORIENTED_EDGE('',*,*,#3494,.F.);
#5158=ORIENTED_EDGE('',*,*,#3602,.F.);
#5159=ORIENTED_EDGE('',*,*,#3806,.T.);
#5160=ORIENTED_EDGE('',*,*,#3701,.T.);
#5161=ORIENTED_EDGE('',*,*,#3492,.F.);
#5162=ORIENTED_EDGE('',*,*,#3601,.F.);
#5163=ORIENTED_EDGE('',*,*,#3807,.F.);
#5164=ORIENTED_EDGE('',*,*,#3702,.F.);
#5165=ORIENTED_EDGE('',*,*,#3806,.F.);
#5166=ORIENTED_EDGE('',*,*,#3703,.T.);
#5167=ORIENTED_EDGE('',*,*,#3807,.T.);
#5168=ORIENTED_EDGE('',*,*,#3600,.F.);
#5169=ORIENTED_EDGE('',*,*,#3385,.T.);
#5170=ORIENTED_EDGE('',*,*,#3700,.T.);
#5171=ORIENTED_EDGE('',*,*,#3808,.T.);
#5172=ORIENTED_EDGE('',*,*,#3603,.F.);
#5173=ORIENTED_EDGE('',*,*,#3490,.F.);
#5174=ORIENTED_EDGE('',*,*,#3606,.F.);
#5175=ORIENTED_EDGE('',*,*,#3381,.T.);
#5176=ORIENTED_EDGE('',*,*,#3697,.T.);
#5177=ORIENTED_EDGE('',*,*,#3488,.F.);
#5178=ORIENTED_EDGE('',*,*,#3698,.T.);
#5179=ORIENTED_EDGE('',*,*,#3383,.T.);
#5180=ORIENTED_EDGE('',*,*,#3605,.F.);
#5181=ORIENTED_EDGE('',*,*,#3809,.T.);
#5182=ORIENTED_EDGE('',*,*,#3604,.F.);
#5183=ORIENTED_EDGE('',*,*,#3808,.F.);
#5184=ORIENTED_EDGE('',*,*,#3699,.F.);
#5185=ORIENTED_EDGE('',*,*,#3809,.F.);
#5186=ORIENTED_EDGE('',*,*,#3696,.T.);
#5187=ORIENTED_EDGE('',*,*,#3810,.T.);
#5188=ORIENTED_EDGE('',*,*,#3607,.F.);
#5189=ORIENTED_EDGE('',*,*,#3486,.F.);
#5190=ORIENTED_EDGE('',*,*,#3610,.F.);
#5191=ORIENTED_EDGE('',*,*,#3377,.T.);
#5192=ORIENTED_EDGE('',*,*,#3693,.T.);
#5193=ORIENTED_EDGE('',*,*,#3484,.F.);
#5194=ORIENTED_EDGE('',*,*,#3694,.T.);
#5195=ORIENTED_EDGE('',*,*,#3379,.T.);
#5196=ORIENTED_EDGE('',*,*,#3609,.F.);
#5197=ORIENTED_EDGE('',*,*,#3811,.T.);
#5198=ORIENTED_EDGE('',*,*,#3608,.F.);
#5199=ORIENTED_EDGE('',*,*,#3810,.F.);
#5200=ORIENTED_EDGE('',*,*,#3695,.F.);
#5201=ORIENTED_EDGE('',*,*,#3811,.F.);
#5202=ORIENTED_EDGE('',*,*,#3692,.T.);
#5203=ORIENTED_EDGE('',*,*,#3812,.T.);
#5204=ORIENTED_EDGE('',*,*,#3611,.F.);
#5205=ORIENTED_EDGE('',*,*,#3482,.F.);
#5206=ORIENTED_EDGE('',*,*,#3614,.F.);
#5207=ORIENTED_EDGE('',*,*,#3373,.T.);
#5208=ORIENTED_EDGE('',*,*,#3689,.T.);
#5209=ORIENTED_EDGE('',*,*,#3476,.F.);
#5210=ORIENTED_EDGE('',*,*,#3690,.T.);
#5211=ORIENTED_EDGE('',*,*,#3375,.T.);
#5212=ORIENTED_EDGE('',*,*,#3613,.F.);
#5213=ORIENTED_EDGE('',*,*,#3813,.T.);
#5214=ORIENTED_EDGE('',*,*,#3612,.F.);
#5215=ORIENTED_EDGE('',*,*,#3812,.F.);
#5216=ORIENTED_EDGE('',*,*,#3691,.F.);
#5217=ORIENTED_EDGE('',*,*,#3813,.F.);
#5218=ORIENTED_EDGE('',*,*,#3684,.T.);
#5219=ORIENTED_EDGE('',*,*,#3814,.T.);
#5220=ORIENTED_EDGE('',*,*,#3619,.F.);
#5221=ORIENTED_EDGE('',*,*,#3480,.F.);
#5222=ORIENTED_EDGE('',*,*,#3622,.F.);
#5223=ORIENTED_EDGE('',*,*,#3369,.T.);
#5224=ORIENTED_EDGE('',*,*,#3681,.T.);
#5225=ORIENTED_EDGE('',*,*,#3472,.F.);
#5226=ORIENTED_EDGE('',*,*,#3682,.T.);
#5227=ORIENTED_EDGE('',*,*,#3371,.T.);
#5228=ORIENTED_EDGE('',*,*,#3621,.F.);
#5229=ORIENTED_EDGE('',*,*,#3815,.T.);
#5230=ORIENTED_EDGE('',*,*,#3620,.F.);
#5231=ORIENTED_EDGE('',*,*,#3814,.F.);
#5232=ORIENTED_EDGE('',*,*,#3683,.F.);
#5233=ORIENTED_EDGE('',*,*,#3815,.F.);
#5234=ORIENTED_EDGE('',*,*,#3688,.T.);
#5235=ORIENTED_EDGE('',*,*,#3816,.T.);
#5236=ORIENTED_EDGE('',*,*,#3615,.F.);
#5237=ORIENTED_EDGE('',*,*,#3474,.F.);
#5238=ORIENTED_EDGE('',*,*,#3618,.F.);
#5239=ORIENTED_EDGE('',*,*,#3365,.T.);
#5240=ORIENTED_EDGE('',*,*,#3685,.T.);
#5241=ORIENTED_EDGE('',*,*,#3478,.F.);
#5242=ORIENTED_EDGE('',*,*,#3686,.T.);
#5243=ORIENTED_EDGE('',*,*,#3367,.T.);
#5244=ORIENTED_EDGE('',*,*,#3617,.F.);
#5245=ORIENTED_EDGE('',*,*,#3817,.T.);
#5246=ORIENTED_EDGE('',*,*,#3616,.F.);
#5247=ORIENTED_EDGE('',*,*,#3816,.F.);
#5248=ORIENTED_EDGE('',*,*,#3687,.F.);
#5249=ORIENTED_EDGE('',*,*,#3817,.F.);
#5250=ORIENTED_EDGE('',*,*,#3680,.T.);
#5251=ORIENTED_EDGE('',*,*,#3818,.T.);
#5252=ORIENTED_EDGE('',*,*,#3623,.F.);
#5253=ORIENTED_EDGE('',*,*,#3470,.F.);
#5254=ORIENTED_EDGE('',*,*,#3678,.T.);
#5255=ORIENTED_EDGE('',*,*,#3360,.T.);
#5256=ORIENTED_EDGE('',*,*,#3625,.F.);
#5257=ORIENTED_EDGE('',*,*,#3819,.T.);
#5258=ORIENTED_EDGE('',*,*,#3624,.F.);
#5259=ORIENTED_EDGE('',*,*,#3818,.F.);
#5260=ORIENTED_EDGE('',*,*,#3679,.F.);
#5261=ORIENTED_EDGE('',*,*,#3819,.F.);
#5262=ORIENTED_EDGE('',*,*,#3677,.T.);
#5263=ORIENTED_EDGE('',*,*,#3820,.T.);
#5264=ORIENTED_EDGE('',*,*,#3626,.F.);
#5265=ORIENTED_EDGE('',*,*,#3467,.F.);
#5266=ORIENTED_EDGE('',*,*,#3675,.T.);
#5267=ORIENTED_EDGE('',*,*,#3353,.T.);
#5268=ORIENTED_EDGE('',*,*,#3628,.F.);
#5269=ORIENTED_EDGE('',*,*,#3821,.T.);
#5270=ORIENTED_EDGE('',*,*,#3627,.F.);
#5271=ORIENTED_EDGE('',*,*,#3820,.F.);
#5272=ORIENTED_EDGE('',*,*,#3676,.F.);
#5273=ORIENTED_EDGE('',*,*,#3821,.F.);
#5274=ORIENTED_EDGE('',*,*,#3582,.F.);
#5275=ORIENTED_EDGE('',*,*,#3822,.T.);
#5276=ORIENTED_EDGE('',*,*,#3721,.T.);
#5277=ORIENTED_EDGE('',*,*,#3502,.F.);
#5278=ORIENTED_EDGE('',*,*,#3581,.F.);
#5279=ORIENTED_EDGE('',*,*,#3823,.F.);
#5280=ORIENTED_EDGE('',*,*,#3722,.F.);
#5281=ORIENTED_EDGE('',*,*,#3822,.F.);
#5282=ORIENTED_EDGE('',*,*,#3723,.T.);
#5283=ORIENTED_EDGE('',*,*,#3823,.T.);
#5284=ORIENTED_EDGE('',*,*,#3580,.F.);
#5285=ORIENTED_EDGE('',*,*,#3344,.T.);
#5286=ORIENTED_EDGE('',*,*,#3579,.F.);
#5287=ORIENTED_EDGE('',*,*,#3824,.T.);
#5288=ORIENTED_EDGE('',*,*,#3724,.T.);
#5289=ORIENTED_EDGE('',*,*,#3464,.F.);
#5290=ORIENTED_EDGE('',*,*,#3578,.F.);
#5291=ORIENTED_EDGE('',*,*,#3825,.F.);
#5292=ORIENTED_EDGE('',*,*,#3725,.F.);
#5293=ORIENTED_EDGE('',*,*,#3824,.F.);
#5294=ORIENTED_EDGE('',*,*,#3726,.T.);
#5295=ORIENTED_EDGE('',*,*,#3825,.T.);
#5296=ORIENTED_EDGE('',*,*,#3577,.F.);
#5297=ORIENTED_EDGE('',*,*,#3337,.T.);
#5298=ORIENTED_EDGE('',*,*,#3731,.T.);
#5299=ORIENTED_EDGE('',*,*,#3826,.T.);
#5300=ORIENTED_EDGE('',*,*,#3572,.F.);
#5301=ORIENTED_EDGE('',*,*,#3459,.F.);
#5302=ORIENTED_EDGE('',*,*,#3576,.F.);
#5303=ORIENTED_EDGE('',*,*,#3827,.T.);
#5304=ORIENTED_EDGE('',*,*,#3727,.T.);
#5305=ORIENTED_EDGE('',*,*,#3461,.F.);
#5306=ORIENTED_EDGE('',*,*,#3575,.F.);
#5307=ORIENTED_EDGE('',*,*,#3828,.F.);
#5308=ORIENTED_EDGE('',*,*,#3728,.F.);
#5309=ORIENTED_EDGE('',*,*,#3827,.F.);
#5310=ORIENTED_EDGE('',*,*,#3729,.T.);
#5311=ORIENTED_EDGE('',*,*,#3828,.T.);
#5312=ORIENTED_EDGE('',*,*,#3574,.F.);
#5313=ORIENTED_EDGE('',*,*,#3829,.T.);
#5314=ORIENTED_EDGE('',*,*,#3573,.F.);
#5315=ORIENTED_EDGE('',*,*,#3826,.F.);
#5316=ORIENTED_EDGE('',*,*,#3730,.F.);
#5317=ORIENTED_EDGE('',*,*,#3829,.F.);
#5318=ORIENTED_EDGE('',*,*,#3736,.T.);
#5319=ORIENTED_EDGE('',*,*,#3830,.T.);
#5320=ORIENTED_EDGE('',*,*,#3567,.F.);
#5321=ORIENTED_EDGE('',*,*,#3455,.F.);
#5322=ORIENTED_EDGE('',*,*,#3571,.F.);
#5323=ORIENTED_EDGE('',*,*,#3831,.T.);
#5324=ORIENTED_EDGE('',*,*,#3732,.T.);
#5325=ORIENTED_EDGE('',*,*,#3457,.F.);
#5326=ORIENTED_EDGE('',*,*,#3570,.F.);
#5327=ORIENTED_EDGE('',*,*,#3832,.F.);
#5328=ORIENTED_EDGE('',*,*,#3733,.F.);
#5329=ORIENTED_EDGE('',*,*,#3831,.F.);
#5330=ORIENTED_EDGE('',*,*,#3734,.T.);
#5331=ORIENTED_EDGE('',*,*,#3832,.T.);
#5332=ORIENTED_EDGE('',*,*,#3569,.F.);
#5333=ORIENTED_EDGE('',*,*,#3833,.T.);
#5334=ORIENTED_EDGE('',*,*,#3568,.F.);
#5335=ORIENTED_EDGE('',*,*,#3830,.F.);
#5336=ORIENTED_EDGE('',*,*,#3735,.F.);
#5337=ORIENTED_EDGE('',*,*,#3833,.F.);
#5338=ORIENTED_EDGE('',*,*,#3751,.T.);
#5339=ORIENTED_EDGE('',*,*,#3834,.T.);
#5340=ORIENTED_EDGE('',*,*,#3552,.F.);
#5341=ORIENTED_EDGE('',*,*,#3451,.F.);
#5342=ORIENTED_EDGE('',*,*,#3556,.F.);
#5343=ORIENTED_EDGE('',*,*,#3835,.T.);
#5344=ORIENTED_EDGE('',*,*,#3747,.T.);
#5345=ORIENTED_EDGE('',*,*,#3443,.F.);
#5346=ORIENTED_EDGE('',*,*,#3555,.F.);
#5347=ORIENTED_EDGE('',*,*,#3836,.F.);
#5348=ORIENTED_EDGE('',*,*,#3748,.F.);
#5349=ORIENTED_EDGE('',*,*,#3835,.F.);
#5350=ORIENTED_EDGE('',*,*,#3749,.T.);
#5351=ORIENTED_EDGE('',*,*,#3836,.T.);
#5352=ORIENTED_EDGE('',*,*,#3554,.F.);
#5353=ORIENTED_EDGE('',*,*,#3837,.T.);
#5354=ORIENTED_EDGE('',*,*,#3553,.F.);
#5355=ORIENTED_EDGE('',*,*,#3834,.F.);
#5356=ORIENTED_EDGE('',*,*,#3750,.F.);
#5357=ORIENTED_EDGE('',*,*,#3837,.F.);
#5358=ORIENTED_EDGE('',*,*,#3756,.T.);
#5359=ORIENTED_EDGE('',*,*,#3838,.T.);
#5360=ORIENTED_EDGE('',*,*,#3547,.F.);
#5361=ORIENTED_EDGE('',*,*,#3447,.F.);
#5362=ORIENTED_EDGE('',*,*,#3551,.F.);
#5363=ORIENTED_EDGE('',*,*,#3839,.T.);
#5364=ORIENTED_EDGE('',*,*,#3752,.T.);
#5365=ORIENTED_EDGE('',*,*,#3449,.F.);
#5366=ORIENTED_EDGE('',*,*,#3550,.F.);
#5367=ORIENTED_EDGE('',*,*,#3840,.F.);
#5368=ORIENTED_EDGE('',*,*,#3753,.F.);
#5369=ORIENTED_EDGE('',*,*,#3839,.F.);
#5370=ORIENTED_EDGE('',*,*,#3754,.T.);
#5371=ORIENTED_EDGE('',*,*,#3840,.T.);
#5372=ORIENTED_EDGE('',*,*,#3549,.F.);
#5373=ORIENTED_EDGE('',*,*,#3841,.T.);
#5374=ORIENTED_EDGE('',*,*,#3548,.F.);
#5375=ORIENTED_EDGE('',*,*,#3838,.F.);
#5376=ORIENTED_EDGE('',*,*,#3755,.F.);
#5377=ORIENTED_EDGE('',*,*,#3841,.F.);
#5378=ORIENTED_EDGE('',*,*,#3746,.T.);
#5379=ORIENTED_EDGE('',*,*,#3842,.T.);
#5380=ORIENTED_EDGE('',*,*,#3557,.F.);
#5381=ORIENTED_EDGE('',*,*,#3441,.F.);
#5382=ORIENTED_EDGE('',*,*,#3561,.F.);
#5383=ORIENTED_EDGE('',*,*,#3843,.T.);
#5384=ORIENTED_EDGE('',*,*,#3742,.T.);
#5385=ORIENTED_EDGE('',*,*,#3439,.F.);
#5386=ORIENTED_EDGE('',*,*,#3560,.F.);
#5387=ORIENTED_EDGE('',*,*,#3844,.F.);
#5388=ORIENTED_EDGE('',*,*,#3743,.F.);
#5389=ORIENTED_EDGE('',*,*,#3843,.F.);
#5390=ORIENTED_EDGE('',*,*,#3744,.T.);
#5391=ORIENTED_EDGE('',*,*,#3844,.T.);
#5392=ORIENTED_EDGE('',*,*,#3559,.F.);
#5393=ORIENTED_EDGE('',*,*,#3845,.T.);
#5394=ORIENTED_EDGE('',*,*,#3558,.F.);
#5395=ORIENTED_EDGE('',*,*,#3842,.F.);
#5396=ORIENTED_EDGE('',*,*,#3745,.F.);
#5397=ORIENTED_EDGE('',*,*,#3845,.F.);
#5398=ORIENTED_EDGE('',*,*,#3741,.T.);
#5399=ORIENTED_EDGE('',*,*,#3846,.T.);
#5400=ORIENTED_EDGE('',*,*,#3562,.F.);
#5401=ORIENTED_EDGE('',*,*,#3437,.F.);
#5402=ORIENTED_EDGE('',*,*,#3566,.F.);
#5403=ORIENTED_EDGE('',*,*,#3847,.T.);
#5404=ORIENTED_EDGE('',*,*,#3737,.T.);
#5405=ORIENTED_EDGE('',*,*,#3453,.F.);
#5406=ORIENTED_EDGE('',*,*,#3565,.F.);
#5407=ORIENTED_EDGE('',*,*,#3848,.F.);
#5408=ORIENTED_EDGE('',*,*,#3738,.F.);
#5409=ORIENTED_EDGE('',*,*,#3847,.F.);
#5410=ORIENTED_EDGE('',*,*,#3739,.T.);
#5411=ORIENTED_EDGE('',*,*,#3848,.T.);
#5412=ORIENTED_EDGE('',*,*,#3564,.F.);
#5413=ORIENTED_EDGE('',*,*,#3849,.T.);
#5414=ORIENTED_EDGE('',*,*,#3563,.F.);
#5415=ORIENTED_EDGE('',*,*,#3846,.F.);
#5416=ORIENTED_EDGE('',*,*,#3740,.F.);
#5417=ORIENTED_EDGE('',*,*,#3849,.F.);
#5418=ORIENTED_EDGE('',*,*,#3761,.T.);
#5419=ORIENTED_EDGE('',*,*,#3850,.T.);
#5420=ORIENTED_EDGE('',*,*,#3542,.F.);
#5421=ORIENTED_EDGE('',*,*,#3435,.F.);
#5422=ORIENTED_EDGE('',*,*,#3546,.F.);
#5423=ORIENTED_EDGE('',*,*,#3851,.T.);
#5424=ORIENTED_EDGE('',*,*,#3757,.T.);
#5425=ORIENTED_EDGE('',*,*,#3445,.F.);
#5426=ORIENTED_EDGE('',*,*,#3545,.F.);
#5427=ORIENTED_EDGE('',*,*,#3852,.F.);
#5428=ORIENTED_EDGE('',*,*,#3758,.F.);
#5429=ORIENTED_EDGE('',*,*,#3851,.F.);
#5430=ORIENTED_EDGE('',*,*,#3759,.T.);
#5431=ORIENTED_EDGE('',*,*,#3852,.T.);
#5432=ORIENTED_EDGE('',*,*,#3544,.F.);
#5433=ORIENTED_EDGE('',*,*,#3853,.T.);
#5434=ORIENTED_EDGE('',*,*,#3543,.F.);
#5435=ORIENTED_EDGE('',*,*,#3850,.F.);
#5436=ORIENTED_EDGE('',*,*,#3760,.F.);
#5437=ORIENTED_EDGE('',*,*,#3853,.F.);
#5438=ORIENTED_EDGE('',*,*,#3766,.T.);
#5439=ORIENTED_EDGE('',*,*,#3854,.T.);
#5440=ORIENTED_EDGE('',*,*,#3537,.F.);
#5441=ORIENTED_EDGE('',*,*,#3405,.F.);
#5442=ORIENTED_EDGE('',*,*,#3541,.F.);
#5443=ORIENTED_EDGE('',*,*,#3855,.T.);
#5444=ORIENTED_EDGE('',*,*,#3762,.T.);
#5445=ORIENTED_EDGE('',*,*,#3433,.F.);
#5446=ORIENTED_EDGE('',*,*,#3540,.F.);
#5447=ORIENTED_EDGE('',*,*,#3856,.F.);
#5448=ORIENTED_EDGE('',*,*,#3763,.F.);
#5449=ORIENTED_EDGE('',*,*,#3855,.F.);
#5450=ORIENTED_EDGE('',*,*,#3764,.T.);
#5451=ORIENTED_EDGE('',*,*,#3856,.T.);
#5452=ORIENTED_EDGE('',*,*,#3539,.F.);
#5453=ORIENTED_EDGE('',*,*,#3857,.T.);
#5454=ORIENTED_EDGE('',*,*,#3538,.F.);
#5455=ORIENTED_EDGE('',*,*,#3854,.F.);
#5456=ORIENTED_EDGE('',*,*,#3765,.F.);
#5457=ORIENTED_EDGE('',*,*,#3857,.F.);
#5458=ORIENTED_EDGE('',*,*,#3771,.T.);
#5459=ORIENTED_EDGE('',*,*,#3858,.T.);
#5460=ORIENTED_EDGE('',*,*,#3532,.F.);
#5461=ORIENTED_EDGE('',*,*,#3431,.F.);
#5462=ORIENTED_EDGE('',*,*,#3536,.F.);
#5463=ORIENTED_EDGE('',*,*,#3859,.T.);
#5464=ORIENTED_EDGE('',*,*,#3767,.T.);
#5465=ORIENTED_EDGE('',*,*,#3407,.F.);
#5466=ORIENTED_EDGE('',*,*,#3535,.F.);
#5467=ORIENTED_EDGE('',*,*,#3860,.F.);
#5468=ORIENTED_EDGE('',*,*,#3768,.F.);
#5469=ORIENTED_EDGE('',*,*,#3859,.F.);
#5470=ORIENTED_EDGE('',*,*,#3769,.T.);
#5471=ORIENTED_EDGE('',*,*,#3860,.T.);
#5472=ORIENTED_EDGE('',*,*,#3534,.F.);
#5473=ORIENTED_EDGE('',*,*,#3861,.T.);
#5474=ORIENTED_EDGE('',*,*,#3533,.F.);
#5475=ORIENTED_EDGE('',*,*,#3858,.F.);
#5476=ORIENTED_EDGE('',*,*,#3770,.F.);
#5477=ORIENTED_EDGE('',*,*,#3861,.F.);
#5478=ORIENTED_EDGE('',*,*,#3776,.T.);
#5479=ORIENTED_EDGE('',*,*,#3862,.T.);
#5480=ORIENTED_EDGE('',*,*,#3527,.F.);
#5481=ORIENTED_EDGE('',*,*,#3427,.F.);
#5482=ORIENTED_EDGE('',*,*,#3531,.F.);
#5483=ORIENTED_EDGE('',*,*,#3863,.T.);
#5484=ORIENTED_EDGE('',*,*,#3772,.T.);
#5485=ORIENTED_EDGE('',*,*,#3429,.F.);
#5486=ORIENTED_EDGE('',*,*,#3530,.F.);
#5487=ORIENTED_EDGE('',*,*,#3864,.F.);
#5488=ORIENTED_EDGE('',*,*,#3773,.F.);
#5489=ORIENTED_EDGE('',*,*,#3863,.F.);
#5490=ORIENTED_EDGE('',*,*,#3774,.T.);
#5491=ORIENTED_EDGE('',*,*,#3864,.T.);
#5492=ORIENTED_EDGE('',*,*,#3529,.F.);
#5493=ORIENTED_EDGE('',*,*,#3865,.T.);
#5494=ORIENTED_EDGE('',*,*,#3528,.F.);
#5495=ORIENTED_EDGE('',*,*,#3862,.F.);
#5496=ORIENTED_EDGE('',*,*,#3775,.F.);
#5497=ORIENTED_EDGE('',*,*,#3865,.F.);
#5498=ORIENTED_EDGE('',*,*,#3663,.T.);
#5499=ORIENTED_EDGE('',*,*,#3866,.T.);
#5500=ORIENTED_EDGE('',*,*,#3640,.F.);
#5501=ORIENTED_EDGE('',*,*,#3421,.F.);
#5502=ORIENTED_EDGE('',*,*,#3644,.F.);
#5503=ORIENTED_EDGE('',*,*,#3867,.T.);
#5504=ORIENTED_EDGE('',*,*,#3659,.T.);
#5505=ORIENTED_EDGE('',*,*,#3419,.F.);
#5506=ORIENTED_EDGE('',*,*,#3643,.F.);
#5507=ORIENTED_EDGE('',*,*,#3868,.F.);
#5508=ORIENTED_EDGE('',*,*,#3660,.F.);
#5509=ORIENTED_EDGE('',*,*,#3867,.F.);
#5510=ORIENTED_EDGE('',*,*,#3661,.T.);
#5511=ORIENTED_EDGE('',*,*,#3868,.T.);
#5512=ORIENTED_EDGE('',*,*,#3642,.F.);
#5513=ORIENTED_EDGE('',*,*,#3869,.T.);
#5514=ORIENTED_EDGE('',*,*,#3641,.F.);
#5515=ORIENTED_EDGE('',*,*,#3866,.F.);
#5516=ORIENTED_EDGE('',*,*,#3662,.F.);
#5517=ORIENTED_EDGE('',*,*,#3869,.F.);
#5518=ORIENTED_EDGE('',*,*,#3658,.T.);
#5519=ORIENTED_EDGE('',*,*,#3870,.T.);
#5520=ORIENTED_EDGE('',*,*,#3645,.F.);
#5521=ORIENTED_EDGE('',*,*,#3417,.F.);
#5522=ORIENTED_EDGE('',*,*,#3649,.F.);
#5523=ORIENTED_EDGE('',*,*,#3871,.T.);
#5524=ORIENTED_EDGE('',*,*,#3654,.T.);
#5525=ORIENTED_EDGE('',*,*,#3411,.F.);
#5526=ORIENTED_EDGE('',*,*,#3648,.F.);
#5527=ORIENTED_EDGE('',*,*,#3872,.F.);
#5528=ORIENTED_EDGE('',*,*,#3655,.F.);
#5529=ORIENTED_EDGE('',*,*,#3871,.F.);
#5530=ORIENTED_EDGE('',*,*,#3656,.T.);
#5531=ORIENTED_EDGE('',*,*,#3872,.T.);
#5532=ORIENTED_EDGE('',*,*,#3647,.F.);
#5533=ORIENTED_EDGE('',*,*,#3873,.T.);
#5534=ORIENTED_EDGE('',*,*,#3646,.F.);
#5535=ORIENTED_EDGE('',*,*,#3870,.F.);
#5536=ORIENTED_EDGE('',*,*,#3657,.F.);
#5537=ORIENTED_EDGE('',*,*,#3873,.F.);
#5538=ORIENTED_EDGE('',*,*,#3781,.T.);
#5539=ORIENTED_EDGE('',*,*,#3874,.T.);
#5540=ORIENTED_EDGE('',*,*,#3522,.F.);
#5541=ORIENTED_EDGE('',*,*,#3415,.F.);
#5542=ORIENTED_EDGE('',*,*,#3526,.F.);
#5543=ORIENTED_EDGE('',*,*,#3875,.T.);
#5544=ORIENTED_EDGE('',*,*,#3777,.T.);
#5545=ORIENTED_EDGE('',*,*,#3425,.F.);
#5546=ORIENTED_EDGE('',*,*,#3525,.F.);
#5547=ORIENTED_EDGE('',*,*,#3876,.F.);
#5548=ORIENTED_EDGE('',*,*,#3778,.F.);
#5549=ORIENTED_EDGE('',*,*,#3875,.F.);
#5550=ORIENTED_EDGE('',*,*,#3779,.T.);
#5551=ORIENTED_EDGE('',*,*,#3876,.T.);
#5552=ORIENTED_EDGE('',*,*,#3524,.F.);
#5553=ORIENTED_EDGE('',*,*,#3877,.T.);
#5554=ORIENTED_EDGE('',*,*,#3523,.F.);
#5555=ORIENTED_EDGE('',*,*,#3874,.F.);
#5556=ORIENTED_EDGE('',*,*,#3780,.F.);
#5557=ORIENTED_EDGE('',*,*,#3877,.F.);
#5558=ORIENTED_EDGE('',*,*,#3653,.T.);
#5559=ORIENTED_EDGE('',*,*,#3878,.T.);
#5560=ORIENTED_EDGE('',*,*,#3517,.F.);
#5561=ORIENTED_EDGE('',*,*,#3409,.F.);
#5562=ORIENTED_EDGE('',*,*,#3521,.F.);
#5563=ORIENTED_EDGE('',*,*,#3879,.T.);
#5564=ORIENTED_EDGE('',*,*,#3782,.T.);
#5565=ORIENTED_EDGE('',*,*,#3413,.F.);
#5566=ORIENTED_EDGE('',*,*,#3520,.F.);
#5567=ORIENTED_EDGE('',*,*,#3880,.F.);
#5568=ORIENTED_EDGE('',*,*,#3783,.F.);
#5569=ORIENTED_EDGE('',*,*,#3879,.F.);
#5570=ORIENTED_EDGE('',*,*,#3784,.T.);
#5571=ORIENTED_EDGE('',*,*,#3880,.T.);
#5572=ORIENTED_EDGE('',*,*,#3519,.F.);
#5573=ORIENTED_EDGE('',*,*,#3881,.T.);
#5574=ORIENTED_EDGE('',*,*,#3518,.F.);
#5575=ORIENTED_EDGE('',*,*,#3878,.F.);
#5576=ORIENTED_EDGE('',*,*,#3785,.F.);
#5577=ORIENTED_EDGE('',*,*,#3881,.F.);
#5578=ORIENTED_EDGE('',*,*,#3786,.T.);
#5579=ORIENTED_EDGE('',*,*,#3333,.F.);
#5580=ORIENTED_EDGE('',*,*,#3650,.F.);
#5581=ORIENTED_EDGE('',*,*,#3882,.T.);
#5582=ORIENTED_EDGE('',*,*,#3787,.T.);
#5583=ORIENTED_EDGE('',*,*,#3882,.F.);
#5584=ORIENTED_EDGE('',*,*,#3652,.F.);
#5585=ORIENTED_EDGE('',*,*,#3883,.T.);
#5586=ORIENTED_EDGE('',*,*,#3788,.T.);
#5587=ORIENTED_EDGE('',*,*,#3883,.F.);
#5588=ORIENTED_EDGE('',*,*,#3651,.F.);
#5589=ORIENTED_EDGE('',*,*,#3335,.T.);
#5590=ORIENTED_EDGE('',*,*,#3884,.T.);
#5591=ORIENTED_EDGE('',*,*,#3885,.T.);
#5592=ORIENTED_EDGE('',*,*,#3886,.F.);
#5593=ORIENTED_EDGE('',*,*,#3885,.F.);
#5594=ORIENTED_EDGE('',*,*,#3887,.F.);
#5595=ORIENTED_EDGE('',*,*,#3888,.T.);
#5596=ORIENTED_EDGE('',*,*,#3889,.T.);
#5597=ORIENTED_EDGE('',*,*,#3890,.T.);
#5598=ORIENTED_EDGE('',*,*,#3891,.F.);
#5599=ORIENTED_EDGE('',*,*,#3892,.F.);
#5600=ORIENTED_EDGE('',*,*,#3893,.T.);
#5601=ORIENTED_EDGE('',*,*,#3894,.F.);
#5602=ORIENTED_EDGE('',*,*,#3895,.T.);
#5603=ORIENTED_EDGE('',*,*,#3896,.T.);
#5604=ORIENTED_EDGE('',*,*,#3897,.F.);
#5605=ORIENTED_EDGE('',*,*,#3896,.F.);
#5606=ORIENTED_EDGE('',*,*,#3898,.T.);
#5607=ORIENTED_EDGE('',*,*,#3899,.T.);
#5608=ORIENTED_EDGE('',*,*,#3900,.T.);
#5609=ORIENTED_EDGE('',*,*,#3901,.T.);
#5610=ORIENTED_EDGE('',*,*,#3902,.T.);
#5611=ORIENTED_EDGE('',*,*,#3887,.T.);
#5612=ORIENTED_EDGE('',*,*,#3903,.T.);
#5613=ORIENTED_EDGE('',*,*,#3904,.T.);
#5614=ORIENTED_EDGE('',*,*,#3905,.T.);
#5615=ORIENTED_EDGE('',*,*,#3906,.T.);
#5616=ORIENTED_EDGE('',*,*,#3907,.T.);
#5617=ORIENTED_EDGE('',*,*,#3884,.F.);
#5618=ORIENTED_EDGE('',*,*,#3895,.F.);
#5619=ORIENTED_EDGE('',*,*,#3908,.F.);
#5620=ORIENTED_EDGE('',*,*,#3909,.T.);
#5621=ORIENTED_EDGE('',*,*,#3910,.F.);
#5622=ORIENTED_EDGE('',*,*,#3911,.F.);
#5623=ORIENTED_EDGE('',*,*,#3912,.T.);
#5624=ORIENTED_EDGE('',*,*,#3889,.F.);
#5625=ORIENTED_EDGE('',*,*,#3913,.F.);
#5626=ORIENTED_EDGE('',*,*,#3914,.F.);
#5627=ORIENTED_EDGE('',*,*,#3915,.F.);
#5628=ORIENTED_EDGE('',*,*,#3916,.F.);
#5629=ORIENTED_EDGE('',*,*,#3917,.T.);
#5630=ORIENTED_EDGE('',*,*,#3918,.F.);
#5631=ORIENTED_EDGE('',*,*,#3919,.F.);
#5632=ORIENTED_EDGE('',*,*,#3893,.F.);
#5633=ORIENTED_EDGE('',*,*,#3920,.F.);
#5634=ORIENTED_EDGE('',*,*,#3921,.F.);
#5635=ORIENTED_EDGE('',*,*,#3922,.F.);
#5636=ORIENTED_EDGE('',*,*,#3897,.T.);
#5637=ORIENTED_EDGE('',*,*,#3886,.T.);
#5638=ORIENTED_EDGE('',*,*,#3923,.T.);
#5639=ORIENTED_EDGE('',*,*,#3924,.T.);
#5640=ORIENTED_EDGE('',*,*,#3891,.T.);
#5641=ORIENTED_EDGE('',*,*,#3925,.F.);
#5642=ORIENTED_EDGE('',*,*,#3926,.T.);
#5643=ORIENTED_EDGE('',*,*,#3927,.T.);
#5644=ORIENTED_EDGE('',*,*,#3902,.F.);
#5645=ORIENTED_EDGE('',*,*,#3928,.T.);
#5646=ORIENTED_EDGE('',*,*,#3908,.T.);
#5647=ORIENTED_EDGE('',*,*,#3888,.F.);
#5648=ORIENTED_EDGE('',*,*,#3924,.F.);
#5649=ORIENTED_EDGE('',*,*,#3929,.F.);
#5650=ORIENTED_EDGE('',*,*,#3920,.T.);
#5651=ORIENTED_EDGE('',*,*,#3892,.T.);
#5652=ORIENTED_EDGE('',*,*,#3919,.T.);
#5653=ORIENTED_EDGE('',*,*,#3930,.F.);
#5654=ORIENTED_EDGE('',*,*,#3903,.F.);
#5655=ORIENTED_EDGE('',*,*,#3894,.T.);
#5656=ORIENTED_EDGE('',*,*,#3931,.T.);
#5657=ORIENTED_EDGE('',*,*,#3925,.T.);
#5658=ORIENTED_EDGE('',*,*,#3890,.F.);
#5659=ORIENTED_EDGE('',*,*,#3912,.F.);
#5660=ORIENTED_EDGE('',*,*,#3918,.T.);
#5661=ORIENTED_EDGE('',*,*,#3932,.T.);
#5662=ORIENTED_EDGE('',*,*,#3904,.F.);
#5663=ORIENTED_EDGE('',*,*,#3930,.T.);
#5664=ORIENTED_EDGE('',*,*,#3906,.F.);
#5665=ORIENTED_EDGE('',*,*,#3933,.T.);
#5666=ORIENTED_EDGE('',*,*,#3916,.T.);
#5667=ORIENTED_EDGE('',*,*,#3934,.F.);
#5668=ORIENTED_EDGE('',*,*,#3915,.T.);
#5669=ORIENTED_EDGE('',*,*,#3935,.F.);
#5670=ORIENTED_EDGE('',*,*,#3907,.F.);
#5671=ORIENTED_EDGE('',*,*,#3934,.T.);
#5672=ORIENTED_EDGE('',*,*,#3914,.T.);
#5673=ORIENTED_EDGE('',*,*,#3936,.F.);
#5674=ORIENTED_EDGE('',*,*,#3937,.T.);
#5675=ORIENTED_EDGE('',*,*,#3938,.F.);
#5676=ORIENTED_EDGE('',*,*,#3939,.F.);
#5677=ORIENTED_EDGE('',*,*,#3940,.T.);
#5678=ORIENTED_EDGE('',*,*,#3898,.F.);
#5679=ORIENTED_EDGE('',*,*,#3935,.T.);
#5680=ORIENTED_EDGE('',*,*,#3938,.T.);
#5681=ORIENTED_EDGE('',*,*,#3941,.T.);
#5682=ORIENTED_EDGE('',*,*,#3942,.F.);
#5683=ORIENTED_EDGE('',*,*,#3943,.F.);
#5684=ORIENTED_EDGE('',*,*,#3910,.T.);
#5685=ORIENTED_EDGE('',*,*,#3944,.F.);
#5686=ORIENTED_EDGE('',*,*,#3900,.F.);
#5687=ORIENTED_EDGE('',*,*,#3945,.F.);
#5688=ORIENTED_EDGE('',*,*,#3946,.F.);
#5689=ORIENTED_EDGE('',*,*,#3942,.T.);
#5690=ORIENTED_EDGE('',*,*,#3947,.T.);
#5691=ORIENTED_EDGE('',*,*,#3948,.T.);
#5692=ORIENTED_EDGE('',*,*,#3922,.T.);
#5693=ORIENTED_EDGE('',*,*,#3949,.T.);
#5694=ORIENTED_EDGE('',*,*,#3927,.F.);
#5695=ORIENTED_EDGE('',*,*,#3950,.F.);
#5696=ORIENTED_EDGE('',*,*,#3926,.F.);
#5697=ORIENTED_EDGE('',*,*,#3931,.F.);
#5698=ORIENTED_EDGE('',*,*,#3911,.T.);
#5699=ORIENTED_EDGE('',*,*,#3950,.T.);
#5700=ORIENTED_EDGE('',*,*,#3909,.F.);
#5701=ORIENTED_EDGE('',*,*,#3928,.F.);
#5702=ORIENTED_EDGE('',*,*,#3901,.F.);
#5703=ORIENTED_EDGE('',*,*,#3944,.T.);
#5704=ORIENTED_EDGE('',*,*,#3923,.F.);
#5705=ORIENTED_EDGE('',*,*,#3949,.F.);
#5706=ORIENTED_EDGE('',*,*,#3921,.T.);
#5707=ORIENTED_EDGE('',*,*,#3929,.T.);
#5708=ORIENTED_EDGE('',*,*,#3899,.F.);
#5709=ORIENTED_EDGE('',*,*,#3940,.F.);
#5710=ORIENTED_EDGE('',*,*,#3951,.T.);
#5711=ORIENTED_EDGE('',*,*,#3945,.T.);
#5712=ORIENTED_EDGE('',*,*,#3951,.F.);
#5713=ORIENTED_EDGE('',*,*,#3939,.T.);
#5714=ORIENTED_EDGE('',*,*,#3943,.T.);
#5715=ORIENTED_EDGE('',*,*,#3946,.T.);
#5716=ORIENTED_EDGE('',*,*,#3913,.T.);
#5717=ORIENTED_EDGE('',*,*,#3948,.F.);
#5718=ORIENTED_EDGE('',*,*,#3952,.F.);
#5719=ORIENTED_EDGE('',*,*,#3936,.T.);
#5720=ORIENTED_EDGE('',*,*,#3952,.T.);
#5721=ORIENTED_EDGE('',*,*,#3947,.F.);
#5722=ORIENTED_EDGE('',*,*,#3941,.F.);
#5723=ORIENTED_EDGE('',*,*,#3937,.F.);
#5724=ORIENTED_EDGE('',*,*,#3905,.F.);
#5725=ORIENTED_EDGE('',*,*,#3932,.F.);
#5726=ORIENTED_EDGE('',*,*,#3917,.F.);
#5727=ORIENTED_EDGE('',*,*,#3933,.F.);
#5728=ORIENTED_EDGE('',*,*,#3953,.T.);
#5729=ORIENTED_EDGE('',*,*,#3954,.T.);
#5730=ORIENTED_EDGE('',*,*,#3955,.F.);
#5731=ORIENTED_EDGE('',*,*,#3956,.T.);
#5732=ORIENTED_EDGE('',*,*,#3957,.T.);
#5733=ORIENTED_EDGE('',*,*,#3958,.F.);
#5734=ORIENTED_EDGE('',*,*,#3959,.F.);
#5735=ORIENTED_EDGE('',*,*,#3960,.T.);
#5736=ORIENTED_EDGE('',*,*,#3961,.T.);
#5737=ORIENTED_EDGE('',*,*,#3962,.F.);
#5738=ORIENTED_EDGE('',*,*,#3963,.F.);
#5739=ORIENTED_EDGE('',*,*,#3954,.F.);
#5740=ORIENTED_EDGE('',*,*,#3964,.T.);
#5741=ORIENTED_EDGE('',*,*,#3965,.T.);
#5742=ORIENTED_EDGE('',*,*,#3966,.F.);
#5743=ORIENTED_EDGE('',*,*,#3965,.F.);
#5744=ORIENTED_EDGE('',*,*,#3959,.T.);
#5745=ORIENTED_EDGE('',*,*,#3967,.T.);
#5746=ORIENTED_EDGE('',*,*,#3968,.F.);
#5747=ORIENTED_EDGE('',*,*,#3969,.T.);
#5748=ORIENTED_EDGE('',*,*,#3968,.T.);
#5749=ORIENTED_EDGE('',*,*,#3970,.T.);
#5750=ORIENTED_EDGE('',*,*,#3971,.F.);
#5751=ORIENTED_EDGE('',*,*,#3972,.F.);
#5752=ORIENTED_EDGE('',*,*,#3966,.T.);
#5753=ORIENTED_EDGE('',*,*,#3953,.F.);
#5754=ORIENTED_EDGE('',*,*,#3973,.T.);
#5755=ORIENTED_EDGE('',*,*,#3974,.T.);
#5756=ORIENTED_EDGE('',*,*,#3975,.T.);
#5757=ORIENTED_EDGE('',*,*,#3976,.T.);
#5758=ORIENTED_EDGE('',*,*,#3964,.F.);
#5759=ORIENTED_EDGE('',*,*,#3977,.T.);
#5760=ORIENTED_EDGE('',*,*,#3978,.F.);
#5761=ORIENTED_EDGE('',*,*,#3973,.F.);
#5762=ORIENTED_EDGE('',*,*,#3979,.T.);
#5763=ORIENTED_EDGE('',*,*,#3980,.T.);
#5764=ORIENTED_EDGE('',*,*,#3981,.F.);
#5765=ORIENTED_EDGE('',*,*,#3974,.F.);
#5766=ORIENTED_EDGE('',*,*,#3978,.T.);
#5767=ORIENTED_EDGE('',*,*,#3982,.T.);
#5768=ORIENTED_EDGE('',*,*,#3983,.F.);
#5769=ORIENTED_EDGE('',*,*,#3975,.F.);
#5770=ORIENTED_EDGE('',*,*,#3981,.T.);
#5771=ORIENTED_EDGE('',*,*,#3984,.T.);
#5772=ORIENTED_EDGE('',*,*,#3979,.F.);
#5773=ORIENTED_EDGE('',*,*,#3976,.F.);
#5774=ORIENTED_EDGE('',*,*,#3983,.T.);
#5775=ORIENTED_EDGE('',*,*,#3977,.F.);
#5776=ORIENTED_EDGE('',*,*,#3984,.F.);
#5777=ORIENTED_EDGE('',*,*,#3982,.F.);
#5778=ORIENTED_EDGE('',*,*,#3980,.F.);
#5779=ORIENTED_EDGE('',*,*,#3985,.F.);
#5780=ORIENTED_EDGE('',*,*,#3986,.T.);
#5781=ORIENTED_EDGE('',*,*,#3955,.T.);
#5782=ORIENTED_EDGE('',*,*,#3963,.T.);
#5783=ORIENTED_EDGE('',*,*,#3987,.T.);
#5784=ORIENTED_EDGE('',*,*,#3988,.F.);
#5785=ORIENTED_EDGE('',*,*,#3989,.F.);
#5786=ORIENTED_EDGE('',*,*,#3985,.T.);
#5787=ORIENTED_EDGE('',*,*,#3990,.T.);
#5788=ORIENTED_EDGE('',*,*,#3991,.F.);
#5789=ORIENTED_EDGE('',*,*,#3957,.F.);
#5790=ORIENTED_EDGE('',*,*,#3992,.F.);
#5791=ORIENTED_EDGE('',*,*,#3988,.T.);
#5792=ORIENTED_EDGE('',*,*,#3993,.F.);
#5793=ORIENTED_EDGE('',*,*,#3961,.F.);
#5794=ORIENTED_EDGE('',*,*,#3994,.F.);
#5795=ORIENTED_EDGE('',*,*,#3971,.T.);
#5796=ORIENTED_EDGE('',*,*,#3993,.T.);
#5797=ORIENTED_EDGE('',*,*,#3990,.F.);
#5798=ORIENTED_EDGE('',*,*,#3987,.F.);
#5799=ORIENTED_EDGE('',*,*,#3962,.T.);
#5800=ORIENTED_EDGE('',*,*,#3994,.T.);
#5801=ORIENTED_EDGE('',*,*,#3960,.F.);
#5802=ORIENTED_EDGE('',*,*,#3969,.F.);
#5803=ORIENTED_EDGE('',*,*,#3972,.T.);
#5804=ORIENTED_EDGE('',*,*,#3991,.T.);
#5805=ORIENTED_EDGE('',*,*,#3970,.F.);
#5806=ORIENTED_EDGE('',*,*,#3967,.F.);
#5807=ORIENTED_EDGE('',*,*,#3958,.T.);
#5808=ORIENTED_EDGE('',*,*,#3992,.T.);
#5809=ORIENTED_EDGE('',*,*,#3956,.F.);
#5810=ORIENTED_EDGE('',*,*,#3986,.F.);
#5811=ORIENTED_EDGE('',*,*,#3989,.T.);
#5812=ORIENTED_EDGE('',*,*,#3995,.T.);
#5813=ORIENTED_EDGE('',*,*,#3996,.T.);
#5814=ORIENTED_EDGE('',*,*,#3997,.F.);
#5815=ORIENTED_EDGE('',*,*,#3998,.F.);
#5816=ORIENTED_EDGE('',*,*,#3999,.F.);
#5817=ORIENTED_EDGE('',*,*,#4000,.T.);
#5818=ORIENTED_EDGE('',*,*,#4001,.T.);
#5819=ORIENTED_EDGE('',*,*,#4002,.F.);
#5820=ORIENTED_EDGE('',*,*,#4003,.T.);
#5821=ORIENTED_EDGE('',*,*,#4004,.T.);
#5822=ORIENTED_EDGE('',*,*,#4005,.F.);
#5823=ORIENTED_EDGE('',*,*,#4004,.F.);
#5824=ORIENTED_EDGE('',*,*,#4006,.T.);
#5825=ORIENTED_EDGE('',*,*,#4007,.T.);
#5826=ORIENTED_EDGE('',*,*,#4008,.F.);
#5827=ORIENTED_EDGE('',*,*,#4007,.F.);
#5828=ORIENTED_EDGE('',*,*,#4009,.F.);
#5829=ORIENTED_EDGE('',*,*,#4010,.T.);
#5830=ORIENTED_EDGE('',*,*,#4011,.T.);
#5831=ORIENTED_EDGE('',*,*,#4012,.F.);
#5832=ORIENTED_EDGE('',*,*,#4013,.F.);
#5833=ORIENTED_EDGE('',*,*,#4014,.F.);
#5834=ORIENTED_EDGE('',*,*,#4015,.F.);
#5835=ORIENTED_EDGE('',*,*,#4011,.F.);
#5836=ORIENTED_EDGE('',*,*,#4008,.T.);
#5837=ORIENTED_EDGE('',*,*,#4005,.T.);
#5838=ORIENTED_EDGE('',*,*,#4016,.T.);
#5839=ORIENTED_EDGE('',*,*,#4017,.T.);
#5840=ORIENTED_EDGE('',*,*,#3997,.T.);
#5841=ORIENTED_EDGE('',*,*,#4018,.T.);
#5842=ORIENTED_EDGE('',*,*,#4013,.T.);
#5843=ORIENTED_EDGE('',*,*,#4010,.F.);
#5844=ORIENTED_EDGE('',*,*,#4019,.F.);
#5845=ORIENTED_EDGE('',*,*,#4020,.T.);
#5846=ORIENTED_EDGE('',*,*,#4015,.T.);
#5847=ORIENTED_EDGE('',*,*,#4021,.F.);
#5848=ORIENTED_EDGE('',*,*,#4022,.F.);
#5849=ORIENTED_EDGE('',*,*,#4012,.T.);
#5850=ORIENTED_EDGE('',*,*,#4014,.T.);
#5851=ORIENTED_EDGE('',*,*,#4020,.F.);
#5852=ORIENTED_EDGE('',*,*,#4023,.F.);
#5853=ORIENTED_EDGE('',*,*,#4021,.T.);
#5854=ORIENTED_EDGE('',*,*,#4019,.T.);
#5855=ORIENTED_EDGE('',*,*,#4009,.T.);
#5856=ORIENTED_EDGE('',*,*,#4022,.T.);
#5857=ORIENTED_EDGE('',*,*,#4023,.T.);
#5858=ORIENTED_EDGE('',*,*,#4001,.F.);
#5859=ORIENTED_EDGE('',*,*,#4024,.F.);
#5860=ORIENTED_EDGE('',*,*,#4025,.F.);
#5861=ORIENTED_EDGE('',*,*,#4026,.F.);
#5862=ORIENTED_EDGE('',*,*,#4003,.F.);
#5863=ORIENTED_EDGE('',*,*,#4006,.F.);
#5864=ORIENTED_EDGE('',*,*,#4024,.T.);
#5865=ORIENTED_EDGE('',*,*,#4000,.F.);
#5866=ORIENTED_EDGE('',*,*,#4027,.F.);
#5867=ORIENTED_EDGE('',*,*,#4028,.T.);
#5868=ORIENTED_EDGE('',*,*,#4025,.T.);
#5869=ORIENTED_EDGE('',*,*,#4028,.F.);
#5870=ORIENTED_EDGE('',*,*,#4029,.F.);
#5871=ORIENTED_EDGE('',*,*,#4030,.T.);
#5872=ORIENTED_EDGE('',*,*,#4026,.T.);
#5873=ORIENTED_EDGE('',*,*,#4030,.F.);
#5874=ORIENTED_EDGE('',*,*,#4031,.F.);
#5875=ORIENTED_EDGE('',*,*,#4002,.T.);
#5876=ORIENTED_EDGE('',*,*,#3999,.T.);
#5877=ORIENTED_EDGE('',*,*,#4031,.T.);
#5878=ORIENTED_EDGE('',*,*,#4029,.T.);
#5879=ORIENTED_EDGE('',*,*,#4027,.T.);
#5880=ORIENTED_EDGE('',*,*,#4016,.F.);
#5881=ORIENTED_EDGE('',*,*,#4032,.F.);
#5882=ORIENTED_EDGE('',*,*,#4033,.T.);
#5883=ORIENTED_EDGE('',*,*,#4034,.T.);
#5884=ORIENTED_EDGE('',*,*,#4017,.F.);
#5885=ORIENTED_EDGE('',*,*,#4034,.F.);
#5886=ORIENTED_EDGE('',*,*,#4035,.T.);
#5887=ORIENTED_EDGE('',*,*,#3998,.T.);
#5888=ORIENTED_EDGE('',*,*,#4018,.F.);
#5889=ORIENTED_EDGE('',*,*,#3996,.F.);
#5890=ORIENTED_EDGE('',*,*,#4036,.T.);
#5891=ORIENTED_EDGE('',*,*,#4032,.T.);
#5892=ORIENTED_EDGE('',*,*,#4033,.F.);
#5893=ORIENTED_EDGE('',*,*,#4036,.F.);
#5894=ORIENTED_EDGE('',*,*,#3995,.F.);
#5895=ORIENTED_EDGE('',*,*,#4035,.F.);
#5896=ORIENTED_EDGE('',*,*,#4037,.T.);
#5897=ORIENTED_EDGE('',*,*,#4038,.T.);
#5898=ORIENTED_EDGE('',*,*,#4039,.F.);
#5899=ORIENTED_EDGE('',*,*,#4040,.T.);
#5900=ORIENTED_EDGE('',*,*,#4041,.T.);
#5901=ORIENTED_EDGE('',*,*,#4042,.F.);
#5902=ORIENTED_EDGE('',*,*,#4043,.F.);
#5903=ORIENTED_EDGE('',*,*,#4044,.T.);
#5904=ORIENTED_EDGE('',*,*,#4045,.T.);
#5905=ORIENTED_EDGE('',*,*,#4046,.F.);
#5906=ORIENTED_EDGE('',*,*,#4047,.F.);
#5907=ORIENTED_EDGE('',*,*,#4038,.F.);
#5908=ORIENTED_EDGE('',*,*,#4048,.F.);
#5909=ORIENTED_EDGE('',*,*,#4049,.T.);
#5910=ORIENTED_EDGE('',*,*,#4050,.F.);
#5911=ORIENTED_EDGE('',*,*,#4049,.F.);
#5912=ORIENTED_EDGE('',*,*,#4043,.T.);
#5913=ORIENTED_EDGE('',*,*,#4051,.T.);
#5914=ORIENTED_EDGE('',*,*,#4052,.F.);
#5915=ORIENTED_EDGE('',*,*,#4053,.T.);
#5916=ORIENTED_EDGE('',*,*,#4052,.T.);
#5917=ORIENTED_EDGE('',*,*,#4054,.T.);
#5918=ORIENTED_EDGE('',*,*,#4055,.F.);
#5919=ORIENTED_EDGE('',*,*,#4056,.F.);
#5920=ORIENTED_EDGE('',*,*,#4050,.T.);
#5921=ORIENTED_EDGE('',*,*,#4037,.F.);
#5922=ORIENTED_EDGE('',*,*,#4057,.F.);
#5923=ORIENTED_EDGE('',*,*,#4058,.T.);
#5924=ORIENTED_EDGE('',*,*,#4039,.T.);
#5925=ORIENTED_EDGE('',*,*,#4047,.T.);
#5926=ORIENTED_EDGE('',*,*,#4059,.T.);
#5927=ORIENTED_EDGE('',*,*,#4060,.F.);
#5928=ORIENTED_EDGE('',*,*,#4061,.F.);
#5929=ORIENTED_EDGE('',*,*,#4057,.T.);
#5930=ORIENTED_EDGE('',*,*,#4062,.T.);
#5931=ORIENTED_EDGE('',*,*,#4063,.F.);
#5932=ORIENTED_EDGE('',*,*,#4041,.F.);
#5933=ORIENTED_EDGE('',*,*,#4064,.F.);
#5934=ORIENTED_EDGE('',*,*,#4060,.T.);
#5935=ORIENTED_EDGE('',*,*,#4065,.F.);
#5936=ORIENTED_EDGE('',*,*,#4045,.F.);
#5937=ORIENTED_EDGE('',*,*,#4066,.F.);
#5938=ORIENTED_EDGE('',*,*,#4055,.T.);
#5939=ORIENTED_EDGE('',*,*,#4065,.T.);
#5940=ORIENTED_EDGE('',*,*,#4062,.F.);
#5941=ORIENTED_EDGE('',*,*,#4059,.F.);
#5942=ORIENTED_EDGE('',*,*,#4046,.T.);
#5943=ORIENTED_EDGE('',*,*,#4066,.T.);
#5944=ORIENTED_EDGE('',*,*,#4044,.F.);
#5945=ORIENTED_EDGE('',*,*,#4053,.F.);
#5946=ORIENTED_EDGE('',*,*,#4056,.T.);
#5947=ORIENTED_EDGE('',*,*,#4063,.T.);
#5948=ORIENTED_EDGE('',*,*,#4054,.F.);
#5949=ORIENTED_EDGE('',*,*,#4051,.F.);
#5950=ORIENTED_EDGE('',*,*,#4042,.T.);
#5951=ORIENTED_EDGE('',*,*,#4064,.T.);
#5952=ORIENTED_EDGE('',*,*,#4040,.F.);
#5953=ORIENTED_EDGE('',*,*,#4058,.F.);
#5954=ORIENTED_EDGE('',*,*,#4061,.T.);
#5955=ORIENTED_EDGE('',*,*,#4067,.F.);
#5956=ORIENTED_EDGE('',*,*,#4068,.F.);
#5957=ORIENTED_EDGE('',*,*,#4069,.F.);
#5958=ORIENTED_EDGE('',*,*,#4070,.F.);
#5959=ORIENTED_EDGE('',*,*,#4048,.T.);
#5960=ORIENTED_EDGE('',*,*,#4067,.T.);
#5961=ORIENTED_EDGE('',*,*,#4071,.F.);
#5962=ORIENTED_EDGE('',*,*,#4072,.F.);
#5963=ORIENTED_EDGE('',*,*,#4073,.T.);
#5964=ORIENTED_EDGE('',*,*,#4070,.T.);
#5965=ORIENTED_EDGE('',*,*,#4074,.F.);
#5966=ORIENTED_EDGE('',*,*,#4075,.F.);
#5967=ORIENTED_EDGE('',*,*,#4071,.T.);
#5968=ORIENTED_EDGE('',*,*,#4069,.T.);
#5969=ORIENTED_EDGE('',*,*,#4076,.F.);
#5970=ORIENTED_EDGE('',*,*,#4077,.F.);
#5971=ORIENTED_EDGE('',*,*,#4074,.T.);
#5972=ORIENTED_EDGE('',*,*,#4068,.T.);
#5973=ORIENTED_EDGE('',*,*,#4073,.F.);
#5974=ORIENTED_EDGE('',*,*,#4078,.F.);
#5975=ORIENTED_EDGE('',*,*,#4076,.T.);
#5976=ORIENTED_EDGE('',*,*,#4072,.T.);
#5977=ORIENTED_EDGE('',*,*,#4075,.T.);
#5978=ORIENTED_EDGE('',*,*,#4077,.T.);
#5979=ORIENTED_EDGE('',*,*,#4078,.T.);
#5980=ORIENTED_EDGE('',*,*,#4079,.F.);
#5981=ORIENTED_EDGE('',*,*,#4080,.F.);
#5982=ORIENTED_EDGE('',*,*,#4081,.T.);
#5983=ORIENTED_EDGE('',*,*,#4082,.F.);
#5984=ORIENTED_EDGE('',*,*,#4081,.F.);
#5985=ORIENTED_EDGE('',*,*,#4083,.T.);
#5986=ORIENTED_EDGE('',*,*,#4084,.T.);
#5987=ORIENTED_EDGE('',*,*,#4085,.F.);
#5988=ORIENTED_EDGE('',*,*,#4086,.F.);
#5989=ORIENTED_EDGE('',*,*,#4079,.T.);
#5990=ORIENTED_EDGE('',*,*,#4080,.T.);
#5991=ORIENTED_EDGE('',*,*,#4087,.T.);
#5992=ORIENTED_EDGE('',*,*,#4088,.F.);
#5993=ORIENTED_EDGE('',*,*,#4087,.F.);
#5994=ORIENTED_EDGE('',*,*,#4089,.T.);
#5995=ORIENTED_EDGE('',*,*,#4090,.F.);
#5996=ORIENTED_EDGE('',*,*,#4091,.T.);
#5997=ORIENTED_EDGE('',*,*,#4092,.T.);
#5998=ORIENTED_EDGE('',*,*,#4093,.T.);
#5999=ORIENTED_EDGE('',*,*,#4092,.F.);
#6000=ORIENTED_EDGE('',*,*,#4094,.T.);
#6001=ORIENTED_EDGE('',*,*,#4095,.T.);
#6002=ORIENTED_EDGE('',*,*,#4096,.T.);
#6003=ORIENTED_EDGE('',*,*,#4097,.F.);
#6004=ORIENTED_EDGE('',*,*,#4098,.T.);
#6005=ORIENTED_EDGE('',*,*,#4099,.T.);
#6006=ORIENTED_EDGE('',*,*,#4096,.F.);
#6007=ORIENTED_EDGE('',*,*,#4100,.T.);
#6008=ORIENTED_EDGE('',*,*,#4101,.T.);
#6009=ORIENTED_EDGE('',*,*,#4102,.T.);
#6010=ORIENTED_EDGE('',*,*,#4089,.F.);
#6011=ORIENTED_EDGE('',*,*,#4103,.T.);
#6012=ORIENTED_EDGE('',*,*,#4085,.T.);
#6013=ORIENTED_EDGE('',*,*,#4104,.T.);
#6014=ORIENTED_EDGE('',*,*,#4088,.T.);
#6015=ORIENTED_EDGE('',*,*,#4105,.F.);
#6016=ORIENTED_EDGE('',*,*,#4106,.F.);
#6017=ORIENTED_EDGE('',*,*,#4107,.F.);
#6018=ORIENTED_EDGE('',*,*,#4094,.F.);
#6019=ORIENTED_EDGE('',*,*,#4091,.F.);
#6020=ORIENTED_EDGE('',*,*,#4108,.F.);
#6021=ORIENTED_EDGE('',*,*,#4083,.F.);
#6022=ORIENTED_EDGE('',*,*,#4109,.F.);
#6023=ORIENTED_EDGE('',*,*,#4098,.F.);
#6024=ORIENTED_EDGE('',*,*,#4101,.F.);
#6025=ORIENTED_EDGE('',*,*,#4110,.F.);
#6026=ORIENTED_EDGE('',*,*,#4106,.T.);
#6027=ORIENTED_EDGE('',*,*,#4111,.T.);
#6028=ORIENTED_EDGE('',*,*,#4102,.F.);
#6029=ORIENTED_EDGE('',*,*,#4111,.F.);
#6030=ORIENTED_EDGE('',*,*,#4105,.T.);
#6031=ORIENTED_EDGE('',*,*,#4097,.T.);
#6032=ORIENTED_EDGE('',*,*,#4103,.F.);
#6033=ORIENTED_EDGE('',*,*,#4099,.F.);
#6034=ORIENTED_EDGE('',*,*,#4109,.T.);
#6035=ORIENTED_EDGE('',*,*,#4086,.T.);
#6036=ORIENTED_EDGE('',*,*,#4104,.F.);
#6037=ORIENTED_EDGE('',*,*,#4084,.F.);
#6038=ORIENTED_EDGE('',*,*,#4108,.T.);
#6039=ORIENTED_EDGE('',*,*,#4090,.T.);
#6040=ORIENTED_EDGE('',*,*,#4100,.F.);
#6041=ORIENTED_EDGE('',*,*,#4095,.F.);
#6042=ORIENTED_EDGE('',*,*,#4107,.T.);
#6043=ORIENTED_EDGE('',*,*,#4110,.T.);
#6044=ORIENTED_EDGE('',*,*,#4082,.T.);
#6045=ORIENTED_EDGE('',*,*,#4093,.F.);
#6046=CYLINDRICAL_SURFACE('',#6754,1.5);
#6047=CYLINDRICAL_SURFACE('',#6757,1.5);
#6048=CYLINDRICAL_SURFACE('',#6760,1.5);
#6049=CYLINDRICAL_SURFACE('',#6763,1.5);
#6050=CYLINDRICAL_SURFACE('',#6771,14.);
#6051=CYLINDRICAL_SURFACE('',#6774,5.);
#6052=CYLINDRICAL_SURFACE('',#6778,5.);
#6053=CYLINDRICAL_SURFACE('',#6781,14.);
#6054=CYLINDRICAL_SURFACE('',#6784,5.);
#6055=CYLINDRICAL_SURFACE('',#6788,5.);
#6056=CYLINDRICAL_SURFACE('',#6798,12.);
#6057=CYLINDRICAL_SURFACE('',#6799,12.);
#6058=CYLINDRICAL_SURFACE('',#6801,3.);
#6059=CYLINDRICAL_SURFACE('',#6804,3.5);
#6060=CYLINDRICAL_SURFACE('',#6807,3.5);
#6061=CYLINDRICAL_SURFACE('',#6810,1.5);
#6062=CYLINDRICAL_SURFACE('',#6813,1.5);
#6063=CYLINDRICAL_SURFACE('',#6816,3.5);
#6064=CYLINDRICAL_SURFACE('',#6829,3.5);
#6065=CYLINDRICAL_SURFACE('',#6831,3.5);
#6066=CYLINDRICAL_SURFACE('',#6837,3.5);
#6067=CYLINDRICAL_SURFACE('',#6843,3.);
#6068=CYLINDRICAL_SURFACE('',#6850,1.5);
#6069=CYLINDRICAL_SURFACE('',#6853,3.5);
#6070=CYLINDRICAL_SURFACE('',#6856,3.);
#6071=CYLINDRICAL_SURFACE('',#6859,3.5);
#6072=CYLINDRICAL_SURFACE('',#6862,3.5);
#6073=CYLINDRICAL_SURFACE('',#6865,1.5);
#6074=CYLINDRICAL_SURFACE('',#6868,1.5);
#6075=CYLINDRICAL_SURFACE('',#6880,3.5);
#6076=CYLINDRICAL_SURFACE('',#6882,3.5);
#6077=CYLINDRICAL_SURFACE('',#6888,3.5);
#6078=CYLINDRICAL_SURFACE('',#6893,3.);
#6079=CYLINDRICAL_SURFACE('',#6900,3.);
#6080=CYLINDRICAL_SURFACE('',#6903,0.27);
#6081=CYLINDRICAL_SURFACE('',#6906,3.68751484013274);
#6082=CYLINDRICAL_SURFACE('',#6909,0.27);
#6083=CYLINDRICAL_SURFACE('',#6912,3.68751484013274);
#6084=CYLINDRICAL_SURFACE('',#6915,0.27);
#6085=CYLINDRICAL_SURFACE('',#6918,3.68751484013274);
#6086=CYLINDRICAL_SURFACE('',#6921,0.269999999999999);
#6087=CYLINDRICAL_SURFACE('',#6924,3.68751484013274);
#6088=CYLINDRICAL_SURFACE('',#6927,0.269999999999999);
#6089=CYLINDRICAL_SURFACE('',#6930,0.269999999999999);
#6090=CYLINDRICAL_SURFACE('',#6933,0.269999999999999);
#6091=CYLINDRICAL_SURFACE('',#6936,0.269999999999999);
#6092=CYLINDRICAL_SURFACE('',#6939,0.269999999999999);
#6093=CYLINDRICAL_SURFACE('',#6942,0.269999999999999);
#6094=CYLINDRICAL_SURFACE('',#6945,0.269999999999999);
#6095=CYLINDRICAL_SURFACE('',#6948,0.269999999999999);
#6096=CYLINDRICAL_SURFACE('',#6951,0.269999999999999);
#6097=CYLINDRICAL_SURFACE('',#6954,0.269999999999999);
#6098=CYLINDRICAL_SURFACE('',#6957,14.4);
#6099=CYLINDRICAL_SURFACE('',#6960,14.4);
#6100=CYLINDRICAL_SURFACE('',#6963,14.4);
#6101=CYLINDRICAL_SURFACE('',#6966,14.4);
#6102=CYLINDRICAL_SURFACE('',#6969,14.4);
#6103=CYLINDRICAL_SURFACE('',#6972,14.4);
#6104=CYLINDRICAL_SURFACE('',#6975,14.4);
#6105=CYLINDRICAL_SURFACE('',#6978,14.4);
#6106=CYLINDRICAL_SURFACE('',#6981,14.4);
#6107=CYLINDRICAL_SURFACE('',#6984,14.4);
#6108=CYLINDRICAL_SURFACE('',#6987,14.4);
#6109=CYLINDRICAL_SURFACE('',#6990,14.4);
#6110=CYLINDRICAL_SURFACE('',#6993,14.4);
#6111=CYLINDRICAL_SURFACE('',#6996,14.4);
#6112=CYLINDRICAL_SURFACE('',#6999,14.4);
#6113=CYLINDRICAL_SURFACE('',#7002,14.4);
#6114=CYLINDRICAL_SURFACE('',#7005,14.4);
#6115=CYLINDRICAL_SURFACE('',#7008,14.4);
#6116=CYLINDRICAL_SURFACE('',#7011,14.4);
#6117=CYLINDRICAL_SURFACE('',#7014,14.4);
#6118=CYLINDRICAL_SURFACE('',#7017,14.4);
#6119=CYLINDRICAL_SURFACE('',#7020,14.4);
#6120=CYLINDRICAL_SURFACE('',#7023,14.4);
#6121=CYLINDRICAL_SURFACE('',#7026,14.4);
#6122=CYLINDRICAL_SURFACE('',#7029,14.4);
#6123=CYLINDRICAL_SURFACE('',#7032,14.4);
#6124=CYLINDRICAL_SURFACE('',#7035,14.4);
#6125=CYLINDRICAL_SURFACE('',#7038,14.4);
#6126=CYLINDRICAL_SURFACE('',#7041,14.4);
#6127=CYLINDRICAL_SURFACE('',#7312,14.4);
#6128=CYLINDRICAL_SURFACE('',#7313,3.68751484013274);
#6129=CYLINDRICAL_SURFACE('',#7314,3.68751484013274);
#6130=CYLINDRICAL_SURFACE('',#7315,12.375);
#6131=CYLINDRICAL_SURFACE('',#7316,0.27);
#6132=CYLINDRICAL_SURFACE('',#7317,0.27);
#6133=CYLINDRICAL_SURFACE('',#7318,3.68751484013274);
#6134=CYLINDRICAL_SURFACE('',#7319,3.68751484013274);
#6135=CYLINDRICAL_SURFACE('',#7320,0.27);
#6136=CYLINDRICAL_SURFACE('',#7321,12.375);
#6137=CYLINDRICAL_SURFACE('',#7322,0.27);
#6138=CYLINDRICAL_SURFACE('',#7323,3.68751484013274);
#6139=CYLINDRICAL_SURFACE('',#7324,3.68751484013274);
#6140=CYLINDRICAL_SURFACE('',#7325,0.269999999999999);
#6141=CYLINDRICAL_SURFACE('',#7326,12.375);
#6142=CYLINDRICAL_SURFACE('',#7327,3.68751484013274);
#6143=CYLINDRICAL_SURFACE('',#7328,3.68751484013274);
#6144=CYLINDRICAL_SURFACE('',#7329,0.269999999999999);
#6145=CYLINDRICAL_SURFACE('',#7330,12.375);
#6146=CYLINDRICAL_SURFACE('',#7331,3.68751484013274);
#6147=CYLINDRICAL_SURFACE('',#7332,3.68751484013274);
#6148=CYLINDRICAL_SURFACE('',#7333,0.269999999999999);
#6149=CYLINDRICAL_SURFACE('',#7334,12.375);
#6150=CYLINDRICAL_SURFACE('',#7335,3.68751484013274);
#6151=CYLINDRICAL_SURFACE('',#7336,3.68751484013274);
#6152=CYLINDRICAL_SURFACE('',#7337,0.269999999999999);
#6153=CYLINDRICAL_SURFACE('',#7338,12.375);
#6154=CYLINDRICAL_SURFACE('',#7339,3.68751484013274);
#6155=CYLINDRICAL_SURFACE('',#7340,3.68751484013274);
#6156=CYLINDRICAL_SURFACE('',#7341,0.269999999999999);
#6157=CYLINDRICAL_SURFACE('',#7342,12.375);
#6158=CYLINDRICAL_SURFACE('',#7343,3.68751484013274);
#6159=CYLINDRICAL_SURFACE('',#7344,3.68751484013274);
#6160=CYLINDRICAL_SURFACE('',#7345,12.375);
#6161=CYLINDRICAL_SURFACE('',#7346,0.269999999999999);
#6162=CYLINDRICAL_SURFACE('',#7347,3.68751484013274);
#6163=CYLINDRICAL_SURFACE('',#7348,3.68751484013274);
#6164=CYLINDRICAL_SURFACE('',#7349,12.375);
#6165=CYLINDRICAL_SURFACE('',#7350,0.269999999999999);
#6166=CYLINDRICAL_SURFACE('',#7351,3.68751484013274);
#6167=CYLINDRICAL_SURFACE('',#7352,3.68751484013274);
#6168=CYLINDRICAL_SURFACE('',#7353,12.375);
#6169=CYLINDRICAL_SURFACE('',#7354,0.269999999999999);
#6170=CYLINDRICAL_SURFACE('',#7355,3.68751484013274);
#6171=CYLINDRICAL_SURFACE('',#7356,3.68751484013274);
#6172=CYLINDRICAL_SURFACE('',#7357,12.375);
#6173=CYLINDRICAL_SURFACE('',#7358,0.27);
#6174=CYLINDRICAL_SURFACE('',#7359,3.68751484013274);
#6175=CYLINDRICAL_SURFACE('',#7360,3.68751484013274);
#6176=CYLINDRICAL_SURFACE('',#7361,12.375);
#6177=CYLINDRICAL_SURFACE('',#7362,0.269999999999999);
#6178=CYLINDRICAL_SURFACE('',#7363,3.68751484013274);
#6179=CYLINDRICAL_SURFACE('',#7364,12.375);
#6180=CYLINDRICAL_SURFACE('',#7365,0.269999999999999);
#6181=CYLINDRICAL_SURFACE('',#7366,3.68751484013274);
#6182=CYLINDRICAL_SURFACE('',#7367,12.375);
#6183=CYLINDRICAL_SURFACE('',#7368,0.27);
#6184=CYLINDRICAL_SURFACE('',#7369,3.68751484013274);
#6185=CYLINDRICAL_SURFACE('',#7370,0.269999999999999);
#6186=CYLINDRICAL_SURFACE('',#7371,12.375);
#6187=CYLINDRICAL_SURFACE('',#7372,3.68751484013274);
#6188=CYLINDRICAL_SURFACE('',#7373,0.27);
#6189=CYLINDRICAL_SURFACE('',#7374,12.375);
#6190=CYLINDRICAL_SURFACE('',#7375,3.68751484013274);
#6191=CYLINDRICAL_SURFACE('',#7376,3.68751484013274);
#6192=CYLINDRICAL_SURFACE('',#7377,0.27);
#6193=CYLINDRICAL_SURFACE('',#7378,12.375);
#6194=CYLINDRICAL_SURFACE('',#7379,0.27);
#6195=CYLINDRICAL_SURFACE('',#7380,3.68751484013274);
#6196=CYLINDRICAL_SURFACE('',#7381,3.68751484013274);
#6197=CYLINDRICAL_SURFACE('',#7382,0.27);
#6198=CYLINDRICAL_SURFACE('',#7383,12.375);
#6199=CYLINDRICAL_SURFACE('',#7384,0.27);
#6200=CYLINDRICAL_SURFACE('',#7385,3.68751484013274);
#6201=CYLINDRICAL_SURFACE('',#7386,3.68751484013274);
#6202=CYLINDRICAL_SURFACE('',#7387,0.269999999999999);
#6203=CYLINDRICAL_SURFACE('',#7388,12.375);
#6204=CYLINDRICAL_SURFACE('',#7389,0.269999999999999);
#6205=CYLINDRICAL_SURFACE('',#7390,3.68751484013274);
#6206=CYLINDRICAL_SURFACE('',#7391,3.68751484013274);
#6207=CYLINDRICAL_SURFACE('',#7392,0.269999999999999);
#6208=CYLINDRICAL_SURFACE('',#7393,12.375);
#6209=CYLINDRICAL_SURFACE('',#7394,0.269999999999999);
#6210=CYLINDRICAL_SURFACE('',#7395,3.68751484013274);
#6211=CYLINDRICAL_SURFACE('',#7396,3.68751484013274);
#6212=CYLINDRICAL_SURFACE('',#7397,0.269999999999999);
#6213=CYLINDRICAL_SURFACE('',#7398,12.375);
#6214=CYLINDRICAL_SURFACE('',#7399,0.269999999999999);
#6215=CYLINDRICAL_SURFACE('',#7400,3.68751484013274);
#6216=CYLINDRICAL_SURFACE('',#7401,3.68751484013274);
#6217=CYLINDRICAL_SURFACE('',#7402,0.27);
#6218=CYLINDRICAL_SURFACE('',#7403,12.375);
#6219=CYLINDRICAL_SURFACE('',#7404,0.269999999999999);
#6220=CYLINDRICAL_SURFACE('',#7405,3.68751484013274);
#6221=CYLINDRICAL_SURFACE('',#7406,3.68751484013274);
#6222=CYLINDRICAL_SURFACE('',#7407,0.269999999999999);
#6223=CYLINDRICAL_SURFACE('',#7408,12.375);
#6224=CYLINDRICAL_SURFACE('',#7409,0.269999999999999);
#6225=CYLINDRICAL_SURFACE('',#7410,3.68751484013274);
#6226=CYLINDRICAL_SURFACE('',#7411,3.68751484013274);
#6227=CYLINDRICAL_SURFACE('',#7412,0.269999999999999);
#6228=CYLINDRICAL_SURFACE('',#7413,12.375);
#6229=CYLINDRICAL_SURFACE('',#7414,0.269999999999999);
#6230=CYLINDRICAL_SURFACE('',#7415,3.68751484013274);
#6231=CYLINDRICAL_SURFACE('',#7416,3.68751484013274);
#6232=CYLINDRICAL_SURFACE('',#7417,0.269999999999999);
#6233=CYLINDRICAL_SURFACE('',#7418,12.375);
#6234=CYLINDRICAL_SURFACE('',#7419,0.269999999999999);
#6235=CYLINDRICAL_SURFACE('',#7420,3.68751484013274);
#6236=CYLINDRICAL_SURFACE('',#7421,3.68751484013274);
#6237=CYLINDRICAL_SURFACE('',#7422,0.269999999999999);
#6238=CYLINDRICAL_SURFACE('',#7423,12.375);
#6239=CYLINDRICAL_SURFACE('',#7424,0.269999999999999);
#6240=CYLINDRICAL_SURFACE('',#7425,3.68751484013274);
#6241=CYLINDRICAL_SURFACE('',#7426,3.68751484013274);
#6242=CYLINDRICAL_SURFACE('',#7427,0.269999999999999);
#6243=CYLINDRICAL_SURFACE('',#7428,12.375);
#6244=CYLINDRICAL_SURFACE('',#7429,0.269999999999999);
#6245=CYLINDRICAL_SURFACE('',#7430,3.68751484013274);
#6246=CYLINDRICAL_SURFACE('',#7431,3.68751484013274);
#6247=CYLINDRICAL_SURFACE('',#7432,0.269999999999999);
#6248=CYLINDRICAL_SURFACE('',#7433,12.375);
#6249=CYLINDRICAL_SURFACE('',#7434,0.269999999999999);
#6250=CYLINDRICAL_SURFACE('',#7435,3.68751484013274);
#6251=CYLINDRICAL_SURFACE('',#7436,3.68751484013274);
#6252=CYLINDRICAL_SURFACE('',#7437,0.269999999999999);
#6253=CYLINDRICAL_SURFACE('',#7438,12.375);
#6254=CYLINDRICAL_SURFACE('',#7439,0.269999999999999);
#6255=CYLINDRICAL_SURFACE('',#7440,3.68751484013274);
#6256=CYLINDRICAL_SURFACE('',#7441,3.68751484013274);
#6257=CYLINDRICAL_SURFACE('',#7442,0.269999999999999);
#6258=CYLINDRICAL_SURFACE('',#7443,12.375);
#6259=CYLINDRICAL_SURFACE('',#7444,0.269999999999999);
#6260=CYLINDRICAL_SURFACE('',#7449,1.5);
#6261=CYLINDRICAL_SURFACE('',#7452,5.);
#6262=CYLINDRICAL_SURFACE('',#7457,1.5);
#6263=CYLINDRICAL_SURFACE('',#7472,5.);
#6264=CYLINDRICAL_SURFACE('',#7485,5.);
#6265=CYLINDRICAL_SURFACE('',#7487,1.25);
#6266=CYLINDRICAL_SURFACE('',#7494,1.5);
#6267=CYLINDRICAL_SURFACE('',#7499,1.5);
#6268=CYLINDRICAL_SURFACE('',#7505,2.5);
#6269=CYLINDRICAL_SURFACE('',#7508,2.5);
#6270=CYLINDRICAL_SURFACE('',#7514,1.5);
#6271=CYLINDRICAL_SURFACE('',#7522,3.5);
#6272=CYLINDRICAL_SURFACE('',#7525,3.5);
#6273=CYLINDRICAL_SURFACE('',#7528,1.5);
#6274=CYLINDRICAL_SURFACE('',#7531,1.5);
#6275=CYLINDRICAL_SURFACE('',#7534,3.5);
#6276=CYLINDRICAL_SURFACE('',#7542,3.5);
#6277=CYLINDRICAL_SURFACE('',#7547,3.5);
#6278=CYLINDRICAL_SURFACE('',#7551,3.5);
#6279=CYLINDRICAL_SURFACE('',#7557,1.25);
#6280=CYLINDRICAL_SURFACE('',#7564,1.5);
#6281=CYLINDRICAL_SURFACE('',#7569,1.5);
#6282=CYLINDRICAL_SURFACE('',#7574,1.5);
#6283=CYLINDRICAL_SURFACE('',#7584,2.5);
#6284=CYLINDRICAL_SURFACE('',#7587,2.5);
#6285=CYLINDRICAL_SURFACE('',#7597,1.25);
#6286=CYLINDRICAL_SURFACE('',#7600,2.5);
#6287=CYLINDRICAL_SURFACE('',#7602,1.5);
#6288=CYLINDRICAL_SURFACE('',#7614,1.25);
#6289=ADVANCED_FACE('',(#319),#6046,.F.);
#6290=ADVANCED_FACE('',(#320),#6047,.F.);
#6291=ADVANCED_FACE('',(#321),#6048,.F.);
#6292=ADVANCED_FACE('',(#322),#6049,.F.);
#6293=ADVANCED_FACE('',(#323),#209,.F.);
#6294=ADVANCED_FACE('',(#324),#210,.F.);
#6295=ADVANCED_FACE('',(#325),#211,.T.);
#6296=ADVANCED_FACE('',(#326),#212,.F.);
#6297=ADVANCED_FACE('',(#327),#213,.F.);
#6298=ADVANCED_FACE('',(#328),#6050,.F.);
#6299=ADVANCED_FACE('',(#329),#6051,.T.);
#6300=ADVANCED_FACE('',(#330),#214,.T.);
#6301=ADVANCED_FACE('',(#331),#6052,.T.);
#6302=ADVANCED_FACE('',(#332),#6053,.F.);
#6303=ADVANCED_FACE('',(#333),#6054,.T.);
#6304=ADVANCED_FACE('',(#334),#215,.F.);
#6305=ADVANCED_FACE('',(#335),#6055,.T.);
#6306=ADVANCED_FACE('',(#336),#216,.F.);
#6307=ADVANCED_FACE('',(#337,#164,#165,#166,#167,#168,#169),#217,.T.);
#6308=ADVANCED_FACE('',(#338,#170,#171,#172,#173,#174,#175),#218,.F.);
#6309=ADVANCED_FACE('',(#339),#6056,.T.);
#6310=ADVANCED_FACE('',(#340),#6057,.T.);
#6311=ADVANCED_FACE('',(#341),#6058,.T.);
#6312=ADVANCED_FACE('',(#342),#6059,.T.);
#6313=ADVANCED_FACE('',(#343),#6060,.T.);
#6314=ADVANCED_FACE('',(#344),#6061,.F.);
#6315=ADVANCED_FACE('',(#345),#6062,.F.);
#6316=ADVANCED_FACE('',(#346),#6063,.T.);
#6317=ADVANCED_FACE('',(#347,#176,#177),#219,.T.);
#6318=ADVANCED_FACE('',(#348,#178,#179,#180),#220,.F.);
#6319=ADVANCED_FACE('',(#349),#221,.F.);
#6320=ADVANCED_FACE('',(#350),#6064,.T.);
#6321=ADVANCED_FACE('',(#351),#222,.F.);
#6322=ADVANCED_FACE('',(#352),#6065,.T.);
#6323=ADVANCED_FACE('',(#353),#223,.F.);
#6324=ADVANCED_FACE('',(#354),#224,.F.);
#6325=ADVANCED_FACE('',(#355),#225,.T.);
#6326=ADVANCED_FACE('',(#356),#226,.T.);
#6327=ADVANCED_FACE('',(#357),#6066,.T.);
#6328=ADVANCED_FACE('',(#358),#227,.T.);
#6329=ADVANCED_FACE('',(#359),#228,.T.);
#6330=ADVANCED_FACE('',(#360),#229,.F.);
#6331=ADVANCED_FACE('',(#361),#230,.T.);
#6332=ADVANCED_FACE('',(#362),#6067,.T.);
#6333=ADVANCED_FACE('',(#363),#231,.F.);
#6334=ADVANCED_FACE('',(#364),#232,.F.);
#6335=ADVANCED_FACE('',(#365,#181),#233,.T.);
#6336=ADVANCED_FACE('',(#366,#182),#234,.T.);
#6337=ADVANCED_FACE('',(#367),#6068,.F.);
#6338=ADVANCED_FACE('',(#368),#6069,.T.);
#6339=ADVANCED_FACE('',(#369),#6070,.T.);
#6340=ADVANCED_FACE('',(#370),#6071,.T.);
#6341=ADVANCED_FACE('',(#371),#6072,.T.);
#6342=ADVANCED_FACE('',(#372),#6073,.F.);
#6343=ADVANCED_FACE('',(#373),#6074,.F.);
#6344=ADVANCED_FACE('',(#374,#183),#235,.T.);
#6345=ADVANCED_FACE('',(#375,#184,#185),#236,.T.);
#6346=ADVANCED_FACE('',(#376,#186,#187,#188,#189),#237,.F.);
#6347=ADVANCED_FACE('',(#377),#238,.F.);
#6348=ADVANCED_FACE('',(#378),#6075,.T.);
#6349=ADVANCED_FACE('',(#379),#239,.F.);
#6350=ADVANCED_FACE('',(#380),#6076,.T.);
#6351=ADVANCED_FACE('',(#381),#240,.F.);
#6352=ADVANCED_FACE('',(#382),#241,.F.);
#6353=ADVANCED_FACE('',(#383),#242,.T.);
#6354=ADVANCED_FACE('',(#384),#243,.T.);
#6355=ADVANCED_FACE('',(#385),#6077,.T.);
#6356=ADVANCED_FACE('',(#386),#244,.T.);
#6357=ADVANCED_FACE('',(#387),#245,.T.);
#6358=ADVANCED_FACE('',(#388),#246,.T.);
#6359=ADVANCED_FACE('',(#389),#6078,.T.);
#6360=ADVANCED_FACE('',(#390),#247,.F.);
#6361=ADVANCED_FACE('',(#391),#248,.F.);
#6362=ADVANCED_FACE('',(#392,#190),#249,.T.);
#6363=ADVANCED_FACE('',(#393,#191),#250,.T.);
#6364=ADVANCED_FACE('',(#394),#6079,.F.);
#6365=ADVANCED_FACE('',(#395),#6080,.F.);
#6366=ADVANCED_FACE('',(#396),#6081,.T.);
#6367=ADVANCED_FACE('',(#397),#6082,.F.);
#6368=ADVANCED_FACE('',(#398),#6083,.T.);
#6369=ADVANCED_FACE('',(#399),#6084,.F.);
#6370=ADVANCED_FACE('',(#400),#6085,.T.);
#6371=ADVANCED_FACE('',(#401),#6086,.F.);
#6372=ADVANCED_FACE('',(#402),#6087,.T.);
#6373=ADVANCED_FACE('',(#403),#6088,.F.);
#6374=ADVANCED_FACE('',(#404),#6089,.F.);
#6375=ADVANCED_FACE('',(#405),#6090,.F.);
#6376=ADVANCED_FACE('',(#406),#6091,.F.);
#6377=ADVANCED_FACE('',(#407),#6092,.F.);
#6378=ADVANCED_FACE('',(#408),#6093,.F.);
#6379=ADVANCED_FACE('',(#409),#6094,.F.);
#6380=ADVANCED_FACE('',(#410),#6095,.F.);
#6381=ADVANCED_FACE('',(#411),#6096,.F.);
#6382=ADVANCED_FACE('',(#412),#6097,.F.);
#6383=ADVANCED_FACE('',(#413),#6098,.T.);
#6384=ADVANCED_FACE('',(#414),#6099,.T.);
#6385=ADVANCED_FACE('',(#415),#6100,.T.);
#6386=ADVANCED_FACE('',(#416),#6101,.T.);
#6387=ADVANCED_FACE('',(#417),#6102,.T.);
#6388=ADVANCED_FACE('',(#418),#6103,.T.);
#6389=ADVANCED_FACE('',(#419),#6104,.T.);
#6390=ADVANCED_FACE('',(#420),#6105,.T.);
#6391=ADVANCED_FACE('',(#421),#6106,.T.);
#6392=ADVANCED_FACE('',(#422),#6107,.T.);
#6393=ADVANCED_FACE('',(#423),#6108,.T.);
#6394=ADVANCED_FACE('',(#424),#6109,.T.);
#6395=ADVANCED_FACE('',(#425),#6110,.T.);
#6396=ADVANCED_FACE('',(#426),#6111,.T.);
#6397=ADVANCED_FACE('',(#427),#6112,.T.);
#6398=ADVANCED_FACE('',(#428),#6113,.T.);
#6399=ADVANCED_FACE('',(#429),#6114,.T.);
#6400=ADVANCED_FACE('',(#430),#6115,.T.);
#6401=ADVANCED_FACE('',(#431),#6116,.T.);
#6402=ADVANCED_FACE('',(#432),#6117,.T.);
#6403=ADVANCED_FACE('',(#433),#6118,.T.);
#6404=ADVANCED_FACE('',(#434),#6119,.T.);
#6405=ADVANCED_FACE('',(#435),#6120,.T.);
#6406=ADVANCED_FACE('',(#436),#6121,.T.);
#6407=ADVANCED_FACE('',(#437),#6122,.T.);
#6408=ADVANCED_FACE('',(#438),#6123,.T.);
#6409=ADVANCED_FACE('',(#439),#6124,.T.);
#6410=ADVANCED_FACE('',(#440),#6125,.T.);
#6411=ADVANCED_FACE('',(#441),#6126,.T.);
#6412=ADVANCED_FACE('',(#442,#192),#251,.F.);
#6413=ADVANCED_FACE('',(#443,#193),#252,.T.);
#6414=ADVANCED_FACE('',(#444),#6127,.T.);
#6415=ADVANCED_FACE('',(#445),#6128,.T.);
#6416=ADVANCED_FACE('',(#446),#6129,.T.);
#6417=ADVANCED_FACE('',(#447),#6130,.T.);
#6418=ADVANCED_FACE('',(#448),#6131,.F.);
#6419=ADVANCED_FACE('',(#449),#6132,.F.);
#6420=ADVANCED_FACE('',(#450),#6133,.T.);
#6421=ADVANCED_FACE('',(#451),#6134,.T.);
#6422=ADVANCED_FACE('',(#452),#6135,.F.);
#6423=ADVANCED_FACE('',(#453),#6136,.T.);
#6424=ADVANCED_FACE('',(#454),#6137,.F.);
#6425=ADVANCED_FACE('',(#455),#6138,.T.);
#6426=ADVANCED_FACE('',(#456),#6139,.T.);
#6427=ADVANCED_FACE('',(#457),#6140,.F.);
#6428=ADVANCED_FACE('',(#458),#6141,.T.);
#6429=ADVANCED_FACE('',(#459),#6142,.T.);
#6430=ADVANCED_FACE('',(#460),#6143,.T.);
#6431=ADVANCED_FACE('',(#461),#6144,.F.);
#6432=ADVANCED_FACE('',(#462),#6145,.T.);
#6433=ADVANCED_FACE('',(#463),#6146,.T.);
#6434=ADVANCED_FACE('',(#464),#6147,.T.);
#6435=ADVANCED_FACE('',(#465),#6148,.F.);
#6436=ADVANCED_FACE('',(#466),#6149,.T.);
#6437=ADVANCED_FACE('',(#467),#6150,.T.);
#6438=ADVANCED_FACE('',(#468),#6151,.T.);
#6439=ADVANCED_FACE('',(#469),#6152,.F.);
#6440=ADVANCED_FACE('',(#470),#6153,.T.);
#6441=ADVANCED_FACE('',(#471),#6154,.T.);
#6442=ADVANCED_FACE('',(#472),#6155,.T.);
#6443=ADVANCED_FACE('',(#473),#6156,.F.);
#6444=ADVANCED_FACE('',(#474),#6157,.T.);
#6445=ADVANCED_FACE('',(#475),#6158,.T.);
#6446=ADVANCED_FACE('',(#476),#6159,.T.);
#6447=ADVANCED_FACE('',(#477),#6160,.T.);
#6448=ADVANCED_FACE('',(#478),#6161,.F.);
#6449=ADVANCED_FACE('',(#479),#6162,.T.);
#6450=ADVANCED_FACE('',(#480),#6163,.T.);
#6451=ADVANCED_FACE('',(#481),#6164,.T.);
#6452=ADVANCED_FACE('',(#482),#6165,.F.);
#6453=ADVANCED_FACE('',(#483),#6166,.T.);
#6454=ADVANCED_FACE('',(#484),#6167,.T.);
#6455=ADVANCED_FACE('',(#485),#6168,.T.);
#6456=ADVANCED_FACE('',(#486),#6169,.F.);
#6457=ADVANCED_FACE('',(#487),#6170,.T.);
#6458=ADVANCED_FACE('',(#488),#6171,.T.);
#6459=ADVANCED_FACE('',(#489),#6172,.T.);
#6460=ADVANCED_FACE('',(#490),#6173,.F.);
#6461=ADVANCED_FACE('',(#491),#6174,.T.);
#6462=ADVANCED_FACE('',(#492),#6175,.T.);
#6463=ADVANCED_FACE('',(#493),#6176,.T.);
#6464=ADVANCED_FACE('',(#494),#6177,.F.);
#6465=ADVANCED_FACE('',(#495),#6178,.T.);
#6466=ADVANCED_FACE('',(#496),#6179,.T.);
#6467=ADVANCED_FACE('',(#497),#6180,.F.);
#6468=ADVANCED_FACE('',(#498),#6181,.T.);
#6469=ADVANCED_FACE('',(#499),#6182,.T.);
#6470=ADVANCED_FACE('',(#500),#6183,.F.);
#6471=ADVANCED_FACE('',(#501),#6184,.T.);
#6472=ADVANCED_FACE('',(#502),#6185,.F.);
#6473=ADVANCED_FACE('',(#503),#6186,.T.);
#6474=ADVANCED_FACE('',(#504),#6187,.T.);
#6475=ADVANCED_FACE('',(#505),#6188,.F.);
#6476=ADVANCED_FACE('',(#506),#6189,.T.);
#6477=ADVANCED_FACE('',(#507),#6190,.T.);
#6478=ADVANCED_FACE('',(#508),#6191,.T.);
#6479=ADVANCED_FACE('',(#509),#6192,.F.);
#6480=ADVANCED_FACE('',(#510),#6193,.T.);
#6481=ADVANCED_FACE('',(#511),#6194,.F.);
#6482=ADVANCED_FACE('',(#512),#6195,.T.);
#6483=ADVANCED_FACE('',(#513),#6196,.T.);
#6484=ADVANCED_FACE('',(#514),#6197,.F.);
#6485=ADVANCED_FACE('',(#515),#6198,.T.);
#6486=ADVANCED_FACE('',(#516),#6199,.F.);
#6487=ADVANCED_FACE('',(#517),#6200,.T.);
#6488=ADVANCED_FACE('',(#518),#6201,.T.);
#6489=ADVANCED_FACE('',(#519),#6202,.F.);
#6490=ADVANCED_FACE('',(#520),#6203,.T.);
#6491=ADVANCED_FACE('',(#521),#6204,.F.);
#6492=ADVANCED_FACE('',(#522),#6205,.T.);
#6493=ADVANCED_FACE('',(#523),#6206,.T.);
#6494=ADVANCED_FACE('',(#524),#6207,.F.);
#6495=ADVANCED_FACE('',(#525),#6208,.T.);
#6496=ADVANCED_FACE('',(#526),#6209,.F.);
#6497=ADVANCED_FACE('',(#527),#6210,.T.);
#6498=ADVANCED_FACE('',(#528),#6211,.T.);
#6499=ADVANCED_FACE('',(#529),#6212,.F.);
#6500=ADVANCED_FACE('',(#530),#6213,.T.);
#6501=ADVANCED_FACE('',(#531),#6214,.F.);
#6502=ADVANCED_FACE('',(#532),#6215,.T.);
#6503=ADVANCED_FACE('',(#533),#6216,.T.);
#6504=ADVANCED_FACE('',(#534),#6217,.F.);
#6505=ADVANCED_FACE('',(#535),#6218,.T.);
#6506=ADVANCED_FACE('',(#536),#6219,.F.);
#6507=ADVANCED_FACE('',(#537),#6220,.T.);
#6508=ADVANCED_FACE('',(#538),#6221,.T.);
#6509=ADVANCED_FACE('',(#539),#6222,.F.);
#6510=ADVANCED_FACE('',(#540),#6223,.T.);
#6511=ADVANCED_FACE('',(#541),#6224,.F.);
#6512=ADVANCED_FACE('',(#542),#6225,.T.);
#6513=ADVANCED_FACE('',(#543),#6226,.T.);
#6514=ADVANCED_FACE('',(#544),#6227,.F.);
#6515=ADVANCED_FACE('',(#545),#6228,.T.);
#6516=ADVANCED_FACE('',(#546),#6229,.F.);
#6517=ADVANCED_FACE('',(#547),#6230,.T.);
#6518=ADVANCED_FACE('',(#548),#6231,.T.);
#6519=ADVANCED_FACE('',(#549),#6232,.F.);
#6520=ADVANCED_FACE('',(#550),#6233,.T.);
#6521=ADVANCED_FACE('',(#551),#6234,.F.);
#6522=ADVANCED_FACE('',(#552),#6235,.T.);
#6523=ADVANCED_FACE('',(#553),#6236,.T.);
#6524=ADVANCED_FACE('',(#554),#6237,.F.);
#6525=ADVANCED_FACE('',(#555),#6238,.T.);
#6526=ADVANCED_FACE('',(#556),#6239,.F.);
#6527=ADVANCED_FACE('',(#557),#6240,.T.);
#6528=ADVANCED_FACE('',(#558),#6241,.T.);
#6529=ADVANCED_FACE('',(#559),#6242,.F.);
#6530=ADVANCED_FACE('',(#560),#6243,.T.);
#6531=ADVANCED_FACE('',(#561),#6244,.F.);
#6532=ADVANCED_FACE('',(#562),#6245,.T.);
#6533=ADVANCED_FACE('',(#563),#6246,.T.);
#6534=ADVANCED_FACE('',(#564),#6247,.F.);
#6535=ADVANCED_FACE('',(#565),#6248,.T.);
#6536=ADVANCED_FACE('',(#566),#6249,.F.);
#6537=ADVANCED_FACE('',(#567),#6250,.T.);
#6538=ADVANCED_FACE('',(#568),#6251,.T.);
#6539=ADVANCED_FACE('',(#569),#6252,.F.);
#6540=ADVANCED_FACE('',(#570),#6253,.T.);
#6541=ADVANCED_FACE('',(#571),#6254,.F.);
#6542=ADVANCED_FACE('',(#572),#6255,.T.);
#6543=ADVANCED_FACE('',(#573),#6256,.T.);
#6544=ADVANCED_FACE('',(#574),#6257,.F.);
#6545=ADVANCED_FACE('',(#575),#6258,.T.);
#6546=ADVANCED_FACE('',(#576),#6259,.F.);
#6547=ADVANCED_FACE('',(#577),#253,.F.);
#6548=ADVANCED_FACE('',(#578),#254,.F.);
#6549=ADVANCED_FACE('',(#579),#255,.F.);
#6550=ADVANCED_FACE('',(#580),#6260,.F.);
#6551=ADVANCED_FACE('',(#581),#6261,.T.);
#6552=ADVANCED_FACE('',(#582),#6262,.F.);
#6553=ADVANCED_FACE('',(#583,#194,#195),#256,.T.);
#6554=ADVANCED_FACE('',(#584),#257,.T.);
#6555=ADVANCED_FACE('',(#585,#196,#197),#258,.T.);
#6556=ADVANCED_FACE('',(#586),#259,.F.);
#6557=ADVANCED_FACE('',(#587),#260,.F.);
#6558=ADVANCED_FACE('',(#588),#261,.T.);
#6559=ADVANCED_FACE('',(#589),#262,.F.);
#6560=ADVANCED_FACE('',(#590),#263,.F.);
#6561=ADVANCED_FACE('',(#591),#6263,.T.);
#6562=ADVANCED_FACE('',(#592),#264,.T.);
#6563=ADVANCED_FACE('',(#593),#265,.F.);
#6564=ADVANCED_FACE('',(#594),#266,.T.);
#6565=ADVANCED_FACE('',(#595),#267,.T.);
#6566=ADVANCED_FACE('',(#596),#268,.T.);
#6567=ADVANCED_FACE('',(#597),#269,.T.);
#6568=ADVANCED_FACE('',(#598),#270,.F.);
#6569=ADVANCED_FACE('',(#599),#271,.T.);
#6570=ADVANCED_FACE('',(#600),#272,.T.);
#6571=ADVANCED_FACE('',(#601),#273,.T.);
#6572=ADVANCED_FACE('',(#602),#274,.F.);
#6573=ADVANCED_FACE('',(#603),#275,.T.);
#6574=ADVANCED_FACE('',(#604),#6264,.F.);
#6575=ADVANCED_FACE('',(#605),#6265,.T.);
#6576=ADVANCED_FACE('',(#606),#6266,.T.);
#6577=ADVANCED_FACE('',(#607),#276,.F.);
#6578=ADVANCED_FACE('',(#608),#6267,.T.);
#6579=ADVANCED_FACE('',(#609,#198),#277,.T.);
#6580=ADVANCED_FACE('',(#610,#199),#278,.T.);
#6581=ADVANCED_FACE('',(#611),#6268,.T.);
#6582=ADVANCED_FACE('',(#612),#279,.F.);
#6583=ADVANCED_FACE('',(#613),#6269,.T.);
#6584=ADVANCED_FACE('',(#614),#280,.F.);
#6585=ADVANCED_FACE('',(#615),#281,.F.);
#6586=ADVANCED_FACE('',(#616),#282,.F.);
#6587=ADVANCED_FACE('',(#617),#6270,.T.);
#6588=ADVANCED_FACE('',(#618),#283,.T.);
#6589=ADVANCED_FACE('',(#619),#284,.F.);
#6590=ADVANCED_FACE('',(#620),#285,.F.);
#6591=ADVANCED_FACE('',(#621),#286,.F.);
#6592=ADVANCED_FACE('',(#622),#287,.F.);
#6593=ADVANCED_FACE('',(#623),#6271,.T.);
#6594=ADVANCED_FACE('',(#624),#6272,.T.);
#6595=ADVANCED_FACE('',(#625),#6273,.F.);
#6596=ADVANCED_FACE('',(#626),#6274,.F.);
#6597=ADVANCED_FACE('',(#627),#6275,.T.);
#6598=ADVANCED_FACE('',(#628,#200,#201,#202),#288,.F.);
#6599=ADVANCED_FACE('',(#629),#289,.F.);
#6600=ADVANCED_FACE('',(#630),#290,.F.);
#6601=ADVANCED_FACE('',(#631),#6276,.T.);
#6602=ADVANCED_FACE('',(#632,#203,#204,#205),#291,.T.);
#6603=ADVANCED_FACE('',(#633),#292,.F.);
#6604=ADVANCED_FACE('',(#634),#6277,.T.);
#6605=ADVANCED_FACE('',(#635),#293,.F.);
#6606=ADVANCED_FACE('',(#636),#294,.T.);
#6607=ADVANCED_FACE('',(#637),#6278,.T.);
#6608=ADVANCED_FACE('',(#638),#295,.T.);
#6609=ADVANCED_FACE('',(#639),#296,.T.);
#6610=ADVANCED_FACE('',(#640),#297,.T.);
#6611=ADVANCED_FACE('',(#641),#6279,.T.);
#6612=ADVANCED_FACE('',(#642),#6280,.T.);
#6613=ADVANCED_FACE('',(#643),#298,.F.);
#6614=ADVANCED_FACE('',(#644),#6281,.T.);
#6615=ADVANCED_FACE('',(#645,#206),#299,.T.);
#6616=ADVANCED_FACE('',(#646),#300,.F.);
#6617=ADVANCED_FACE('',(#647),#6282,.T.);
#6618=ADVANCED_FACE('',(#648),#301,.T.);
#6619=ADVANCED_FACE('',(#649),#302,.F.);
#6620=ADVANCED_FACE('',(#650),#303,.F.);
#6621=ADVANCED_FACE('',(#651),#304,.F.);
#6622=ADVANCED_FACE('',(#652),#305,.F.);
#6623=ADVANCED_FACE('',(#653,#207),#306,.F.);
#6624=ADVANCED_FACE('',(#654),#6283,.T.);
#6625=ADVANCED_FACE('',(#655),#307,.F.);
#6626=ADVANCED_FACE('',(#656),#6284,.T.);
#6627=ADVANCED_FACE('',(#657),#308,.F.);
#6628=ADVANCED_FACE('',(#658),#309,.T.);
#6629=ADVANCED_FACE('',(#659),#127,.T.);
#6630=ADVANCED_FACE('',(#660),#6285,.F.);
#6631=ADVANCED_FACE('',(#661),#6286,.T.);
#6632=ADVANCED_FACE('',(#662),#6287,.F.);
#6633=ADVANCED_FACE('',(#663),#310,.F.);
#6634=ADVANCED_FACE('',(#664),#311,.F.);
#6635=ADVANCED_FACE('',(#665,#208),#312,.T.);
#6636=ADVANCED_FACE('',(#666),#6288,.F.);
#6637=ADVANCED_FACE('',(#667),#313,.T.);
#6638=ADVANCED_FACE('',(#668),#314,.T.);
#6639=ADVANCED_FACE('',(#669),#315,.T.);
#6640=ADVANCED_FACE('',(#670),#316,.T.);
#6641=ADVANCED_FACE('',(#671),#317,.F.);
#6642=ADVANCED_FACE('',(#672),#318,.F.);
#6643=CLOSED_SHELL('',(#6289,#6290,#6291,#6292,#6293,#6294,#6295,#6296,
#6297,#6298,#6299,#6300,#6301,#6302,#6303,#6304,#6305,#6306,#6307,#6308,
#6309,#6310));
#6644=CLOSED_SHELL('',(#6311,#6312,#6313,#6314,#6315,#6316,#6317,#6318,
#6319,#6320,#6321,#6322,#6323,#6324,#6325,#6326,#6327,#6328,#6329,#6330,
#6331,#6332,#6333,#6334,#6335,#6336));
#6645=CLOSED_SHELL('',(#6337,#6338,#6339,#6340,#6341,#6342,#6343,#6344,
#6345,#6346,#6347,#6348,#6349,#6350,#6351,#6352,#6353,#6354,#6355,#6356,
#6357,#6358,#6359,#6360,#6361,#6362,#6363));
#6646=CLOSED_SHELL('',(#6364,#6365,#6366,#6367,#6368,#6369,#6370,#6371,
#6372,#6373,#6374,#6375,#6376,#6377,#6378,#6379,#6380,#6381,#6382,#6383,
#6384,#6385,#6386,#6387,#6388,#6389,#6390,#6391,#6392,#6393,#6394,#6395,
#6396,#6397,#6398,#6399,#6400,#6401,#6402,#6403,#6404,#6405,#6406,#6407,
#6408,#6409,#6410,#6411,#6412,#6413,#6414,#6415,#6416,#6417,#6418,#6419,
#6420,#6421,#6422,#6423,#6424,#6425,#6426,#6427,#6428,#6429,#6430,#6431,
#6432,#6433,#6434,#6435,#6436,#6437,#6438,#6439,#6440,#6441,#6442,#6443,
#6444,#6445,#6446,#6447,#6448,#6449,#6450,#6451,#6452,#6453,#6454,#6455,
#6456,#6457,#6458,#6459,#6460,#6461,#6462,#6463,#6464,#6465,#6466,#6467,
#6468,#6469,#6470,#6471,#6472,#6473,#6474,#6475,#6476,#6477,#6478,#6479,
#6480,#6481,#6482,#6483,#6484,#6485,#6486,#6487,#6488,#6489,#6490,#6491,
#6492,#6493,#6494,#6495,#6496,#6497,#6498,#6499,#6500,#6501,#6502,#6503,
#6504,#6505,#6506,#6507,#6508,#6509,#6510,#6511,#6512,#6513,#6514,#6515,
#6516,#6517,#6518,#6519,#6520,#6521,#6522,#6523,#6524,#6525,#6526,#6527,
#6528,#6529,#6530,#6531,#6532,#6533,#6534,#6535,#6536,#6537,#6538,#6539,
#6540,#6541,#6542,#6543,#6544,#6545,#6546,#6547,#6548,#6549));
#6647=CLOSED_SHELL('',(#6550,#6551,#6552,#6553,#6554,#6555,#6556,#6557,
#6558,#6559,#6560,#6561,#6562,#6563,#6564,#6565,#6566,#6567,#6568,#6569,
#6570,#6571,#6572,#6573,#6574));
#6648=CLOSED_SHELL('',(#6575,#6576,#6577,#6578,#6579,#6580,#6581,#6582,
#6583,#6584,#6585,#6586,#6587,#6588,#6589,#6590,#6591,#6592));
#6649=CLOSED_SHELL('',(#6593,#6594,#6595,#6596,#6597,#6598,#6599,#6600,
#6601,#6602,#6603,#6604,#6605,#6606,#6607,#6608,#6609,#6610));
#6650=CLOSED_SHELL('',(#6611,#6612,#6613,#6614,#6615,#6616,#6617,#6618,
#6619,#6620,#6621,#6622,#6623,#6624,#6625,#6626,#6627,#6628));
#6651=CLOSED_SHELL('',(#6629,#6630,#6631,#6632,#6633,#6634,#6635,#6636,
#6637,#6638,#6639,#6640,#6641,#6642));
#6652=DERIVED_UNIT_ELEMENT(#6670,1.);
#6653=DERIVED_UNIT_ELEMENT(#11935,-3.);
#6654=DERIVED_UNIT_ELEMENT(#6670,1.);
#6655=DERIVED_UNIT_ELEMENT(#11935,-3.);
#6656=DERIVED_UNIT_ELEMENT(#6670,1.);
#6657=DERIVED_UNIT_ELEMENT(#11935,-3.);
#6658=DERIVED_UNIT_ELEMENT(#6670,1.);
#6659=DERIVED_UNIT_ELEMENT(#11935,-3.);
#6660=DERIVED_UNIT_ELEMENT(#6670,1.);
#6661=DERIVED_UNIT_ELEMENT(#11935,-3.);
#6662=DERIVED_UNIT_ELEMENT(#6670,1.);
#6663=DERIVED_UNIT_ELEMENT(#11935,-3.);
#6664=DERIVED_UNIT_ELEMENT(#6670,1.);
#6665=DERIVED_UNIT_ELEMENT(#11935,-3.);
#6666=DERIVED_UNIT_ELEMENT(#6670,1.);
#6667=DERIVED_UNIT_ELEMENT(#11935,-3.);
#6668=DERIVED_UNIT_ELEMENT(#6670,1.);
#6669=DERIVED_UNIT_ELEMENT(#11935,-3.);
#6670=(
MASS_UNIT()
NAMED_UNIT(*)
SI_UNIT(.KILO.,.GRAM.)
);
#6671=DERIVED_UNIT((#6652,#6653));
#6672=DERIVED_UNIT((#6654,#6655));
#6673=DERIVED_UNIT((#6656,#6657));
#6674=DERIVED_UNIT((#6658,#6659));
#6675=DERIVED_UNIT((#6660,#6661));
#6676=DERIVED_UNIT((#6662,#6663));
#6677=DERIVED_UNIT((#6664,#6665));
#6678=DERIVED_UNIT((#6666,#6667));
#6679=DERIVED_UNIT((#6668,#6669));
#6680=MEASURE_REPRESENTATION_ITEM('density measure',
POSITIVE_RATIO_MEASURE(7850.),#6671);
#6681=MEASURE_REPRESENTATION_ITEM('density measure',
POSITIVE_RATIO_MEASURE(7850.),#6672);
#6682=MEASURE_REPRESENTATION_ITEM('density measure',
POSITIVE_RATIO_MEASURE(7850.),#6673);
#6683=MEASURE_REPRESENTATION_ITEM('density measure',
POSITIVE_RATIO_MEASURE(7850.),#6674);
#6684=MEASURE_REPRESENTATION_ITEM('density measure',
POSITIVE_RATIO_MEASURE(7850.),#6675);
#6685=MEASURE_REPRESENTATION_ITEM('density measure',
POSITIVE_RATIO_MEASURE(7850.),#6676);
#6686=MEASURE_REPRESENTATION_ITEM('density measure',
POSITIVE_RATIO_MEASURE(7850.),#6677);
#6687=MEASURE_REPRESENTATION_ITEM('density measure',
POSITIVE_RATIO_MEASURE(7850.),#6678);
#6688=MEASURE_REPRESENTATION_ITEM('density measure',
POSITIVE_RATIO_MEASURE(7850.),#6679);
#6689=PROPERTY_DEFINITION_REPRESENTATION(#6734,#6707);
#6690=PROPERTY_DEFINITION_REPRESENTATION(#6735,#6708);
#6691=PROPERTY_DEFINITION_REPRESENTATION(#6736,#6709);
#6692=PROPERTY_DEFINITION_REPRESENTATION(#6737,#6710);
#6693=PROPERTY_DEFINITION_REPRESENTATION(#6738,#6711);
#6694=PROPERTY_DEFINITION_REPRESENTATION(#6739,#6712);
#6695=PROPERTY_DEFINITION_REPRESENTATION(#6740,#6713);
#6696=PROPERTY_DEFINITION_REPRESENTATION(#6741,#6714);
#6697=PROPERTY_DEFINITION_REPRESENTATION(#6742,#6715);
#6698=PROPERTY_DEFINITION_REPRESENTATION(#6743,#6716);
#6699=PROPERTY_DEFINITION_REPRESENTATION(#6744,#6717);
#6700=PROPERTY_DEFINITION_REPRESENTATION(#6745,#6718);
#6701=PROPERTY_DEFINITION_REPRESENTATION(#6746,#6719);
#6702=PROPERTY_DEFINITION_REPRESENTATION(#6747,#6720);
#6703=PROPERTY_DEFINITION_REPRESENTATION(#6748,#6721);
#6704=PROPERTY_DEFINITION_REPRESENTATION(#6749,#6722);
#6705=PROPERTY_DEFINITION_REPRESENTATION(#6750,#6723);
#6706=PROPERTY_DEFINITION_REPRESENTATION(#6751,#6724);
#6707=REPRESENTATION('material name',(#6725),#11924);
#6708=REPRESENTATION('density',(#6680),#11924);
#6709=REPRESENTATION('material name',(#6726),#11925);
#6710=REPRESENTATION('density',(#6681),#11925);
#6711=REPRESENTATION('material name',(#6727),#11926);
#6712=REPRESENTATION('density',(#6682),#11926);
#6713=REPRESENTATION('material name',(#6728),#11927);
#6714=REPRESENTATION('density',(#6683),#11927);
#6715=REPRESENTATION('material name',(#6729),#11928);
#6716=REPRESENTATION('density',(#6684),#11928);
#6717=REPRESENTATION('material name',(#6730),#11929);
#6718=REPRESENTATION('density',(#6685),#11929);
#6719=REPRESENTATION('material name',(#6731),#11930);
#6720=REPRESENTATION('density',(#6686),#11930);
#6721=REPRESENTATION('material name',(#6732),#11931);
#6722=REPRESENTATION('density',(#6687),#11931);
#6723=REPRESENTATION('material name',(#6733),#11932);
#6724=REPRESENTATION('density',(#6688),#11932);
#6725=DESCRIPTIVE_REPRESENTATION_ITEM('Steel','Steel');
#6726=DESCRIPTIVE_REPRESENTATION_ITEM('Steel','Steel');
#6727=DESCRIPTIVE_REPRESENTATION_ITEM('Steel','Steel');
#6728=DESCRIPTIVE_REPRESENTATION_ITEM('Steel','Steel');
#6729=DESCRIPTIVE_REPRESENTATION_ITEM('Steel','Steel');
#6730=DESCRIPTIVE_REPRESENTATION_ITEM('Steel','Steel');
#6731=DESCRIPTIVE_REPRESENTATION_ITEM('Steel','Steel');
#6732=DESCRIPTIVE_REPRESENTATION_ITEM('Steel','Steel');
#6733=DESCRIPTIVE_REPRESENTATION_ITEM('Steel','Steel');
#6734=PROPERTY_DEFINITION('material property','material name',#11999);
#6735=PROPERTY_DEFINITION('material property','density of part',#11999);
#6736=PROPERTY_DEFINITION('material property','material name',#12000);
#6737=PROPERTY_DEFINITION('material property','density of part',#12000);
#6738=PROPERTY_DEFINITION('material property','material name',#12001);
#6739=PROPERTY_DEFINITION('material property','density of part',#12001);
#6740=PROPERTY_DEFINITION('material property','material name',#12002);
#6741=PROPERTY_DEFINITION('material property','density of part',#12002);
#6742=PROPERTY_DEFINITION('material property','material name',#12003);
#6743=PROPERTY_DEFINITION('material property','density of part',#12003);
#6744=PROPERTY_DEFINITION('material property','material name',#12004);
#6745=PROPERTY_DEFINITION('material property','density of part',#12004);
#6746=PROPERTY_DEFINITION('material property','material name',#12005);
#6747=PROPERTY_DEFINITION('material property','density of part',#12005);
#6748=PROPERTY_DEFINITION('material property','material name',#12006);
#6749=PROPERTY_DEFINITION('material property','density of part',#12006);
#6750=PROPERTY_DEFINITION('material property','material name',#12007);
#6751=PROPERTY_DEFINITION('material property','density of part',#12007);
#6752=AXIS2_PLACEMENT_3D('',#9908,#7650,#7651);
#6753=AXIS2_PLACEMENT_3D('',#9909,#7652,#7653);
#6754=AXIS2_PLACEMENT_3D('',#9910,#7654,#7655);
#6755=AXIS2_PLACEMENT_3D('',#9912,#7656,#7657);
#6756=AXIS2_PLACEMENT_3D('',#9915,#7659,#7660);
#6757=AXIS2_PLACEMENT_3D('',#9916,#7661,#7662);
#6758=AXIS2_PLACEMENT_3D('',#9918,#7663,#7664);
#6759=AXIS2_PLACEMENT_3D('',#9921,#7666,#7667);
#6760=AXIS2_PLACEMENT_3D('',#9922,#7668,#7669);
#6761=AXIS2_PLACEMENT_3D('',#9924,#7670,#7671);
#6762=AXIS2_PLACEMENT_3D('',#9927,#7673,#7674);
#6763=AXIS2_PLACEMENT_3D('',#9928,#7675,#7676);
#6764=AXIS2_PLACEMENT_3D('',#9930,#7677,#7678);
#6765=AXIS2_PLACEMENT_3D('',#9933,#7680,#7681);
#6766=AXIS2_PLACEMENT_3D('',#9934,#7682,#7683);
#6767=AXIS2_PLACEMENT_3D('',#9943,#7688,#7689);
#6768=AXIS2_PLACEMENT_3D('',#9949,#7693,#7694);
#6769=AXIS2_PLACEMENT_3D('',#9955,#7698,#7699);
#6770=AXIS2_PLACEMENT_3D('',#9961,#7703,#7704);
#6771=AXIS2_PLACEMENT_3D('',#9970,#7709,#7710);
#6772=AXIS2_PLACEMENT_3D('',#9973,#7711,#7712);
#6773=AXIS2_PLACEMENT_3D('',#9977,#7714,#7715);
#6774=AXIS2_PLACEMENT_3D('',#9979,#7717,#7718);
#6775=AXIS2_PLACEMENT_3D('',#9981,#7719,#7720);
#6776=AXIS2_PLACEMENT_3D('',#9984,#7722,#7723);
#6777=AXIS2_PLACEMENT_3D('',#9985,#7724,#7725);
#6778=AXIS2_PLACEMENT_3D('',#9991,#7729,#7730);
#6779=AXIS2_PLACEMENT_3D('',#9994,#7731,#7732);
#6780=AXIS2_PLACEMENT_3D('',#9998,#7734,#7735);
#6781=AXIS2_PLACEMENT_3D('',#10000,#7737,#7738);
#6782=AXIS2_PLACEMENT_3D('',#10002,#7739,#7740);
#6783=AXIS2_PLACEMENT_3D('',#10005,#7742,#7743);
#6784=AXIS2_PLACEMENT_3D('',#10006,#7744,#7745);
#6785=AXIS2_PLACEMENT_3D('',#10008,#7746,#7747);
#6786=AXIS2_PLACEMENT_3D('',#10011,#7749,#7750);
#6787=AXIS2_PLACEMENT_3D('',#10012,#7751,#7752);
#6788=AXIS2_PLACEMENT_3D('',#10018,#7756,#7757);
#6789=AXIS2_PLACEMENT_3D('',#10019,#7758,#7759);
#6790=AXIS2_PLACEMENT_3D('',#10020,#7760,#7761);
#6791=AXIS2_PLACEMENT_3D('',#10021,#7762,#7763);
#6792=AXIS2_PLACEMENT_3D('',#10024,#7766,#7767);
#6793=AXIS2_PLACEMENT_3D('',#10025,#7768,#7769);
#6794=AXIS2_PLACEMENT_3D('',#10026,#7770,#7771);
#6795=AXIS2_PLACEMENT_3D('',#10027,#7772,#7773);
#6796=AXIS2_PLACEMENT_3D('',#10028,#7774,#7775);
#6797=AXIS2_PLACEMENT_3D('',#10029,#7776,#7777);
#6798=AXIS2_PLACEMENT_3D('',#10030,#7778,#7779);
#6799=AXIS2_PLACEMENT_3D('',#10031,#7780,#7781);
#6800=AXIS2_PLACEMENT_3D('',#10032,#7782,#7783);
#6801=AXIS2_PLACEMENT_3D('',#10033,#7784,#7785);
#6802=AXIS2_PLACEMENT_3D('',#10035,#7786,#7787);
#6803=AXIS2_PLACEMENT_3D('',#10038,#7789,#7790);
#6804=AXIS2_PLACEMENT_3D('',#10039,#7791,#7792);
#6805=AXIS2_PLACEMENT_3D('',#10042,#7793,#7794);
#6806=AXIS2_PLACEMENT_3D('',#10046,#7796,#7797);
#6807=AXIS2_PLACEMENT_3D('',#10048,#7799,#7800);
#6808=AXIS2_PLACEMENT_3D('',#10051,#7801,#7802);
#6809=AXIS2_PLACEMENT_3D('',#10055,#7804,#7805);
#6810=AXIS2_PLACEMENT_3D('',#10057,#7807,#7808);
#6811=AXIS2_PLACEMENT_3D('',#10059,#7809,#7810);
#6812=AXIS2_PLACEMENT_3D('',#10062,#7812,#7813);
#6813=AXIS2_PLACEMENT_3D('',#10063,#7814,#7815);
#6814=AXIS2_PLACEMENT_3D('',#10065,#7816,#7817);
#6815=AXIS2_PLACEMENT_3D('',#10068,#7819,#7820);
#6816=AXIS2_PLACEMENT_3D('',#10069,#7821,#7822);
#6817=AXIS2_PLACEMENT_3D('',#10072,#7823,#7824);
#6818=AXIS2_PLACEMENT_3D('',#10074,#7825,#7826);
#6819=AXIS2_PLACEMENT_3D('',#10078,#7828,#7829);
#6820=AXIS2_PLACEMENT_3D('',#10081,#7831,#7832);
#6821=AXIS2_PLACEMENT_3D('',#10082,#7833,#7834);
#6822=AXIS2_PLACEMENT_3D('',#10085,#7835,#7836);
#6823=AXIS2_PLACEMENT_3D('',#10090,#7839,#7840);
#6824=AXIS2_PLACEMENT_3D('',#10095,#7843,#7844);
#6825=AXIS2_PLACEMENT_3D('',#10098,#7847,#7848);
#6826=AXIS2_PLACEMENT_3D('',#10102,#7850,#7851);
#6827=AXIS2_PLACEMENT_3D('',#10107,#7854,#7855);
#6828=AXIS2_PLACEMENT_3D('',#10109,#7857,#7858);
#6829=AXIS2_PLACEMENT_3D('',#10111,#7860,#7861);
#6830=AXIS2_PLACEMENT_3D('',#10113,#7863,#7864);
#6831=AXIS2_PLACEMENT_3D('',#10114,#7865,#7866);
#6832=AXIS2_PLACEMENT_3D('',#10118,#7868,#7869);
#6833=AXIS2_PLACEMENT_3D('',#10120,#7871,#7872);
#6834=AXIS2_PLACEMENT_3D('',#10122,#7874,#7875);
#6835=AXIS2_PLACEMENT_3D('',#10124,#7877,#7878);
#6836=AXIS2_PLACEMENT_3D('',#10125,#7879,#7880);
#6837=AXIS2_PLACEMENT_3D('',#10129,#7883,#7884);
#6838=AXIS2_PLACEMENT_3D('',#10131,#7885,#7886);
#6839=AXIS2_PLACEMENT_3D('',#10133,#7888,#7889);
#6840=AXIS2_PLACEMENT_3D('',#10135,#7891,#7892);
#6841=AXIS2_PLACEMENT_3D('',#10136,#7893,#7894);
#6842=AXIS2_PLACEMENT_3D('',#10142,#7898,#7899);
#6843=AXIS2_PLACEMENT_3D('',#10148,#7903,#7904);
#6844=AXIS2_PLACEMENT_3D('',#10151,#7906,#7907);
#6845=AXIS2_PLACEMENT_3D('',#10152,#7908,#7909);
#6846=AXIS2_PLACEMENT_3D('',#10156,#7912,#7913);
#6847=AXIS2_PLACEMENT_3D('',#10158,#7915,#7916);
#6848=AXIS2_PLACEMENT_3D('',#10159,#7917,#7918);
#6849=AXIS2_PLACEMENT_3D('',#10160,#7919,#7920);
#6850=AXIS2_PLACEMENT_3D('',#10161,#7921,#7922);
#6851=AXIS2_PLACEMENT_3D('',#10163,#7923,#7924);
#6852=AXIS2_PLACEMENT_3D('',#10166,#7926,#7927);
#6853=AXIS2_PLACEMENT_3D('',#10167,#7928,#7929);
#6854=AXIS2_PLACEMENT_3D('',#10170,#7930,#7931);
#6855=AXIS2_PLACEMENT_3D('',#10174,#7933,#7934);
#6856=AXIS2_PLACEMENT_3D('',#10176,#7936,#7937);
#6857=AXIS2_PLACEMENT_3D('',#10178,#7938,#7939);
#6858=AXIS2_PLACEMENT_3D('',#10181,#7941,#7942);
#6859=AXIS2_PLACEMENT_3D('',#10182,#7943,#7944);
#6860=AXIS2_PLACEMENT_3D('',#10185,#7945,#7946);
#6861=AXIS2_PLACEMENT_3D('',#10189,#7948,#7949);
#6862=AXIS2_PLACEMENT_3D('',#10191,#7951,#7952);
#6863=AXIS2_PLACEMENT_3D('',#10194,#7953,#7954);
#6864=AXIS2_PLACEMENT_3D('',#10198,#7956,#7957);
#6865=AXIS2_PLACEMENT_3D('',#10200,#7959,#7960);
#6866=AXIS2_PLACEMENT_3D('',#10202,#7961,#7962);
#6867=AXIS2_PLACEMENT_3D('',#10205,#7964,#7965);
#6868=AXIS2_PLACEMENT_3D('',#10206,#7966,#7967);
#6869=AXIS2_PLACEMENT_3D('',#10208,#7968,#7969);
#6870=AXIS2_PLACEMENT_3D('',#10211,#7971,#7972);
#6871=AXIS2_PLACEMENT_3D('',#10212,#7973,#7974);
#6872=AXIS2_PLACEMENT_3D('',#10218,#7978,#7979);
#6873=AXIS2_PLACEMENT_3D('',#10221,#7980,#7981);
#6874=AXIS2_PLACEMENT_3D('',#10229,#7985,#7986);
#6875=AXIS2_PLACEMENT_3D('',#10237,#7990,#7991);
#6876=AXIS2_PLACEMENT_3D('',#10240,#7994,#7995);
#6877=AXIS2_PLACEMENT_3D('',#10245,#7998,#7999);
#6878=AXIS2_PLACEMENT_3D('',#10249,#8001,#8002);
#6879=AXIS2_PLACEMENT_3D('',#10251,#8004,#8005);
#6880=AXIS2_PLACEMENT_3D('',#10254,#8008,#8009);
#6881=AXIS2_PLACEMENT_3D('',#10256,#8011,#8012);
#6882=AXIS2_PLACEMENT_3D('',#10258,#8014,#8015);
#6883=AXIS2_PLACEMENT_3D('',#10262,#8017,#8018);
#6884=AXIS2_PLACEMENT_3D('',#10264,#8020,#8021);
#6885=AXIS2_PLACEMENT_3D('',#10266,#8023,#8024);
#6886=AXIS2_PLACEMENT_3D('',#10268,#8026,#8027);
#6887=AXIS2_PLACEMENT_3D('',#10269,#8028,#8029);
#6888=AXIS2_PLACEMENT_3D('',#10273,#8032,#8033);
#6889=AXIS2_PLACEMENT_3D('',#10275,#8034,#8035);
#6890=AXIS2_PLACEMENT_3D('',#10277,#8037,#8038);
#6891=AXIS2_PLACEMENT_3D('',#10279,#8040,#8041);
#6892=AXIS2_PLACEMENT_3D('',#10280,#8042,#8043);
#6893=AXIS2_PLACEMENT_3D('',#10286,#8047,#8048);
#6894=AXIS2_PLACEMENT_3D('',#10289,#8050,#8051);
#6895=AXIS2_PLACEMENT_3D('',#10290,#8052,#8053);
#6896=AXIS2_PLACEMENT_3D('',#10294,#8056,#8057);
#6897=AXIS2_PLACEMENT_3D('',#10296,#8059,#8060);
#6898=AXIS2_PLACEMENT_3D('',#10297,#8061,#8062);
#6899=AXIS2_PLACEMENT_3D('',#10298,#8063,#8064);
#6900=AXIS2_PLACEMENT_3D('',#10299,#8065,#8066);
#6901=AXIS2_PLACEMENT_3D('',#10302,#8067,#8068);
#6902=AXIS2_PLACEMENT_3D('',#10306,#8070,#8071);
#6903=AXIS2_PLACEMENT_3D('',#10308,#8073,#8074);
#6904=AXIS2_PLACEMENT_3D('',#10311,#8075,#8076);
#6905=AXIS2_PLACEMENT_3D('',#10315,#8078,#8079);
#6906=AXIS2_PLACEMENT_3D('',#10317,#8081,#8082);
#6907=AXIS2_PLACEMENT_3D('',#10319,#8083,#8084);
#6908=AXIS2_PLACEMENT_3D('',#10322,#8086,#8087);
#6909=AXIS2_PLACEMENT_3D('',#10323,#8088,#8089);
#6910=AXIS2_PLACEMENT_3D('',#10326,#8090,#8091);
#6911=AXIS2_PLACEMENT_3D('',#10330,#8093,#8094);
#6912=AXIS2_PLACEMENT_3D('',#10332,#8096,#8097);
#6913=AXIS2_PLACEMENT_3D('',#10334,#8098,#8099);
#6914=AXIS2_PLACEMENT_3D('',#10337,#8101,#8102);
#6915=AXIS2_PLACEMENT_3D('',#10338,#8103,#8104);
#6916=AXIS2_PLACEMENT_3D('',#10341,#8105,#8106);
#6917=AXIS2_PLACEMENT_3D('',#10345,#8108,#8109);
#6918=AXIS2_PLACEMENT_3D('',#10347,#8111,#8112);
#6919=AXIS2_PLACEMENT_3D('',#10349,#8113,#8114);
#6920=AXIS2_PLACEMENT_3D('',#10351,#8115,#8116);
#6921=AXIS2_PLACEMENT_3D('',#10353,#8118,#8119);
#6922=AXIS2_PLACEMENT_3D('',#10356,#8120,#8121);
#6923=AXIS2_PLACEMENT_3D('',#10360,#8123,#8124);
#6924=AXIS2_PLACEMENT_3D('',#10362,#8126,#8127);
#6925=AXIS2_PLACEMENT_3D('',#10364,#8128,#8129);
#6926=AXIS2_PLACEMENT_3D('',#10366,#8130,#8131);
#6927=AXIS2_PLACEMENT_3D('',#10368,#8133,#8134);
#6928=AXIS2_PLACEMENT_3D('',#10371,#8135,#8136);
#6929=AXIS2_PLACEMENT_3D('',#10375,#8138,#8139);
#6930=AXIS2_PLACEMENT_3D('',#10377,#8141,#8142);
#6931=AXIS2_PLACEMENT_3D('',#10380,#8143,#8144);
#6932=AXIS2_PLACEMENT_3D('',#10384,#8146,#8147);
#6933=AXIS2_PLACEMENT_3D('',#10386,#8149,#8150);
#6934=AXIS2_PLACEMENT_3D('',#10389,#8151,#8152);
#6935=AXIS2_PLACEMENT_3D('',#10393,#8154,#8155);
#6936=AXIS2_PLACEMENT_3D('',#10395,#8157,#8158);
#6937=AXIS2_PLACEMENT_3D('',#10398,#8159,#8160);
#6938=AXIS2_PLACEMENT_3D('',#10402,#8162,#8163);
#6939=AXIS2_PLACEMENT_3D('',#10404,#8165,#8166);
#6940=AXIS2_PLACEMENT_3D('',#10407,#8167,#8168);
#6941=AXIS2_PLACEMENT_3D('',#10411,#8170,#8171);
#6942=AXIS2_PLACEMENT_3D('',#10413,#8173,#8174);
#6943=AXIS2_PLACEMENT_3D('',#10416,#8175,#8176);
#6944=AXIS2_PLACEMENT_3D('',#10420,#8178,#8179);
#6945=AXIS2_PLACEMENT_3D('',#10422,#8181,#8182);
#6946=AXIS2_PLACEMENT_3D('',#10425,#8183,#8184);
#6947=AXIS2_PLACEMENT_3D('',#10429,#8186,#8187);
#6948=AXIS2_PLACEMENT_3D('',#10431,#8189,#8190);
#6949=AXIS2_PLACEMENT_3D('',#10434,#8191,#8192);
#6950=AXIS2_PLACEMENT_3D('',#10438,#8194,#8195);
#6951=AXIS2_PLACEMENT_3D('',#10440,#8197,#8198);
#6952=AXIS2_PLACEMENT_3D('',#10443,#8199,#8200);
#6953=AXIS2_PLACEMENT_3D('',#10447,#8202,#8203);
#6954=AXIS2_PLACEMENT_3D('',#10449,#8205,#8206);
#6955=AXIS2_PLACEMENT_3D('',#10452,#8207,#8208);
#6956=AXIS2_PLACEMENT_3D('',#10456,#8210,#8211);
#6957=AXIS2_PLACEMENT_3D('',#10458,#8213,#8214);
#6958=AXIS2_PLACEMENT_3D('',#10461,#8215,#8216);
#6959=AXIS2_PLACEMENT_3D('',#10465,#8218,#8219);
#6960=AXIS2_PLACEMENT_3D('',#10467,#8221,#8222);
#6961=AXIS2_PLACEMENT_3D('',#10470,#8223,#8224);
#6962=AXIS2_PLACEMENT_3D('',#10474,#8226,#8227);
#6963=AXIS2_PLACEMENT_3D('',#10476,#8229,#8230);
#6964=AXIS2_PLACEMENT_3D('',#10479,#8231,#8232);
#6965=AXIS2_PLACEMENT_3D('',#10483,#8234,#8235);
#6966=AXIS2_PLACEMENT_3D('',#10485,#8237,#8238);
#6967=AXIS2_PLACEMENT_3D('',#10488,#8239,#8240);
#6968=AXIS2_PLACEMENT_3D('',#10492,#8242,#8243);
#6969=AXIS2_PLACEMENT_3D('',#10494,#8245,#8246);
#6970=AXIS2_PLACEMENT_3D('',#10497,#8247,#8248);
#6971=AXIS2_PLACEMENT_3D('',#10501,#8250,#8251);
#6972=AXIS2_PLACEMENT_3D('',#10503,#8253,#8254);
#6973=AXIS2_PLACEMENT_3D('',#10506,#8255,#8256);
#6974=AXIS2_PLACEMENT_3D('',#10510,#8258,#8259);
#6975=AXIS2_PLACEMENT_3D('',#10512,#8261,#8262);
#6976=AXIS2_PLACEMENT_3D('',#10515,#8263,#8264);
#6977=AXIS2_PLACEMENT_3D('',#10519,#8266,#8267);
#6978=AXIS2_PLACEMENT_3D('',#10521,#8269,#8270);
#6979=AXIS2_PLACEMENT_3D('',#10524,#8271,#8272);
#6980=AXIS2_PLACEMENT_3D('',#10528,#8274,#8275);
#6981=AXIS2_PLACEMENT_3D('',#10530,#8277,#8278);
#6982=AXIS2_PLACEMENT_3D('',#10533,#8279,#8280);
#6983=AXIS2_PLACEMENT_3D('',#10537,#8282,#8283);
#6984=AXIS2_PLACEMENT_3D('',#10539,#8285,#8286);
#6985=AXIS2_PLACEMENT_3D('',#10542,#8287,#8288);
#6986=AXIS2_PLACEMENT_3D('',#10546,#8290,#8291);
#6987=AXIS2_PLACEMENT_3D('',#10548,#8293,#8294);
#6988=AXIS2_PLACEMENT_3D('',#10551,#8295,#8296);
#6989=AXIS2_PLACEMENT_3D('',#10555,#8298,#8299);
#6990=AXIS2_PLACEMENT_3D('',#10557,#8301,#8302);
#6991=AXIS2_PLACEMENT_3D('',#10560,#8303,#8304);
#6992=AXIS2_PLACEMENT_3D('',#10564,#8306,#8307);
#6993=AXIS2_PLACEMENT_3D('',#10566,#8309,#8310);
#6994=AXIS2_PLACEMENT_3D('',#10569,#8311,#8312);
#6995=AXIS2_PLACEMENT_3D('',#10573,#8314,#8315);
#6996=AXIS2_PLACEMENT_3D('',#10575,#8317,#8318);
#6997=AXIS2_PLACEMENT_3D('',#10578,#8319,#8320);
#6998=AXIS2_PLACEMENT_3D('',#10582,#8322,#8323);
#6999=AXIS2_PLACEMENT_3D('',#10584,#8325,#8326);
#7000=AXIS2_PLACEMENT_3D('',#10586,#8327,#8328);
#7001=AXIS2_PLACEMENT_3D('',#10589,#8330,#8331);
#7002=AXIS2_PLACEMENT_3D('',#10590,#8332,#8333);
#7003=AXIS2_PLACEMENT_3D('',#10592,#8334,#8335);
#7004=AXIS2_PLACEMENT_3D('',#10595,#8337,#8338);
#7005=AXIS2_PLACEMENT_3D('',#10596,#8339,#8340);
#7006=AXIS2_PLACEMENT_3D('',#10598,#8341,#8342);
#7007=AXIS2_PLACEMENT_3D('',#10601,#8344,#8345);
#7008=AXIS2_PLACEMENT_3D('',#10602,#8346,#8347);
#7009=AXIS2_PLACEMENT_3D('',#10605,#8348,#8349);
#7010=AXIS2_PLACEMENT_3D('',#10609,#8351,#8352);
#7011=AXIS2_PLACEMENT_3D('',#10611,#8354,#8355);
#7012=AXIS2_PLACEMENT_3D('',#10614,#8356,#8357);
#7013=AXIS2_PLACEMENT_3D('',#10618,#8359,#8360);
#7014=AXIS2_PLACEMENT_3D('',#10620,#8362,#8363);
#7015=AXIS2_PLACEMENT_3D('',#10623,#8364,#8365);
#7016=AXIS2_PLACEMENT_3D('',#10627,#8367,#8368);
#7017=AXIS2_PLACEMENT_3D('',#10629,#8370,#8371);
#7018=AXIS2_PLACEMENT_3D('',#10632,#8372,#8373);
#7019=AXIS2_PLACEMENT_3D('',#10636,#8375,#8376);
#7020=AXIS2_PLACEMENT_3D('',#10638,#8378,#8379);
#7021=AXIS2_PLACEMENT_3D('',#10641,#8380,#8381);
#7022=AXIS2_PLACEMENT_3D('',#10645,#8383,#8384);
#7023=AXIS2_PLACEMENT_3D('',#10647,#8386,#8387);
#7024=AXIS2_PLACEMENT_3D('',#10650,#8388,#8389);
#7025=AXIS2_PLACEMENT_3D('',#10654,#8391,#8392);
#7026=AXIS2_PLACEMENT_3D('',#10656,#8394,#8395);
#7027=AXIS2_PLACEMENT_3D('',#10659,#8396,#8397);
#7028=AXIS2_PLACEMENT_3D('',#10663,#8399,#8400);
#7029=AXIS2_PLACEMENT_3D('',#10665,#8402,#8403);
#7030=AXIS2_PLACEMENT_3D('',#10668,#8404,#8405);
#7031=AXIS2_PLACEMENT_3D('',#10672,#8407,#8408);
#7032=AXIS2_PLACEMENT_3D('',#10674,#8410,#8411);
#7033=AXIS2_PLACEMENT_3D('',#10677,#8412,#8413);
#7034=AXIS2_PLACEMENT_3D('',#10681,#8415,#8416);
#7035=AXIS2_PLACEMENT_3D('',#10683,#8418,#8419);
#7036=AXIS2_PLACEMENT_3D('',#10686,#8420,#8421);
#7037=AXIS2_PLACEMENT_3D('',#10690,#8423,#8424);
#7038=AXIS2_PLACEMENT_3D('',#10692,#8426,#8427);
#7039=AXIS2_PLACEMENT_3D('',#10695,#8428,#8429);
#7040=AXIS2_PLACEMENT_3D('',#10699,#8431,#8432);
#7041=AXIS2_PLACEMENT_3D('',#10701,#8434,#8435);
#7042=AXIS2_PLACEMENT_3D('',#10704,#8436,#8437);
#7043=AXIS2_PLACEMENT_3D('',#10708,#8439,#8440);
#7044=AXIS2_PLACEMENT_3D('',#10710,#8442,#8443);
#7045=AXIS2_PLACEMENT_3D('',#10712,#8444,#8445);
#7046=AXIS2_PLACEMENT_3D('',#10714,#8446,#8447);
#7047=AXIS2_PLACEMENT_3D('',#10716,#8448,#8449);
#7048=AXIS2_PLACEMENT_3D('',#10718,#8450,#8451);
#7049=AXIS2_PLACEMENT_3D('',#10719,#8452,#8453);
#7050=AXIS2_PLACEMENT_3D('',#10721,#8454,#8455);
#7051=AXIS2_PLACEMENT_3D('',#10723,#8456,#8457);
#7052=AXIS2_PLACEMENT_3D('',#10725,#8458,#8459);
#7053=AXIS2_PLACEMENT_3D('',#10727,#8460,#8461);
#7054=AXIS2_PLACEMENT_3D('',#10728,#8462,#8463);
#7055=AXIS2_PLACEMENT_3D('',#10730,#8464,#8465);
#7056=AXIS2_PLACEMENT_3D('',#10732,#8466,#8467);
#7057=AXIS2_PLACEMENT_3D('',#10734,#8468,#8469);
#7058=AXIS2_PLACEMENT_3D('',#10736,#8470,#8471);
#7059=AXIS2_PLACEMENT_3D('',#10737,#8472,#8473);
#7060=AXIS2_PLACEMENT_3D('',#10739,#8474,#8475);
#7061=AXIS2_PLACEMENT_3D('',#10741,#8476,#8477);
#7062=AXIS2_PLACEMENT_3D('',#10743,#8478,#8479);
#7063=AXIS2_PLACEMENT_3D('',#10745,#8480,#8481);
#7064=AXIS2_PLACEMENT_3D('',#10746,#8482,#8483);
#7065=AXIS2_PLACEMENT_3D('',#10748,#8484,#8485);
#7066=AXIS2_PLACEMENT_3D('',#10750,#8486,#8487);
#7067=AXIS2_PLACEMENT_3D('',#10752,#8488,#8489);
#7068=AXIS2_PLACEMENT_3D('',#10754,#8490,#8491);
#7069=AXIS2_PLACEMENT_3D('',#10755,#8492,#8493);
#7070=AXIS2_PLACEMENT_3D('',#10757,#8494,#8495);
#7071=AXIS2_PLACEMENT_3D('',#10759,#8496,#8497);
#7072=AXIS2_PLACEMENT_3D('',#10761,#8498,#8499);
#7073=AXIS2_PLACEMENT_3D('',#10763,#8500,#8501);
#7074=AXIS2_PLACEMENT_3D('',#10764,#8502,#8503);
#7075=AXIS2_PLACEMENT_3D('',#10766,#8504,#8505);
#7076=AXIS2_PLACEMENT_3D('',#10768,#8506,#8507);
#7077=AXIS2_PLACEMENT_3D('',#10770,#8508,#8509);
#7078=AXIS2_PLACEMENT_3D('',#10772,#8510,#8511);
#7079=AXIS2_PLACEMENT_3D('',#10773,#8512,#8513);
#7080=AXIS2_PLACEMENT_3D('',#10775,#8514,#8515);
#7081=AXIS2_PLACEMENT_3D('',#10777,#8516,#8517);
#7082=AXIS2_PLACEMENT_3D('',#10779,#8518,#8519);
#7083=AXIS2_PLACEMENT_3D('',#10781,#8520,#8521);
#7084=AXIS2_PLACEMENT_3D('',#10782,#8522,#8523);
#7085=AXIS2_PLACEMENT_3D('',#10784,#8524,#8525);
#7086=AXIS2_PLACEMENT_3D('',#10786,#8526,#8527);
#7087=AXIS2_PLACEMENT_3D('',#10788,#8528,#8529);
#7088=AXIS2_PLACEMENT_3D('',#10790,#8530,#8531);
#7089=AXIS2_PLACEMENT_3D('',#10791,#8532,#8533);
#7090=AXIS2_PLACEMENT_3D('',#10793,#8534,#8535);
#7091=AXIS2_PLACEMENT_3D('',#10795,#8536,#8537);
#7092=AXIS2_PLACEMENT_3D('',#10797,#8538,#8539);
#7093=AXIS2_PLACEMENT_3D('',#10799,#8540,#8541);
#7094=AXIS2_PLACEMENT_3D('',#10800,#8542,#8543);
#7095=AXIS2_PLACEMENT_3D('',#10802,#8544,#8545);
#7096=AXIS2_PLACEMENT_3D('',#10804,#8546,#8547);
#7097=AXIS2_PLACEMENT_3D('',#10806,#8548,#8549);
#7098=AXIS2_PLACEMENT_3D('',#10808,#8550,#8551);
#7099=AXIS2_PLACEMENT_3D('',#10809,#8552,#8553);
#7100=AXIS2_PLACEMENT_3D('',#10811,#8554,#8555);
#7101=AXIS2_PLACEMENT_3D('',#10813,#8556,#8557);
#7102=AXIS2_PLACEMENT_3D('',#10815,#8558,#8559);
#7103=AXIS2_PLACEMENT_3D('',#10817,#8560,#8561);
#7104=AXIS2_PLACEMENT_3D('',#10818,#8562,#8563);
#7105=AXIS2_PLACEMENT_3D('',#10820,#8564,#8565);
#7106=AXIS2_PLACEMENT_3D('',#10822,#8566,#8567);
#7107=AXIS2_PLACEMENT_3D('',#10823,#8568,#8569);
#7108=AXIS2_PLACEMENT_3D('',#10825,#8570,#8571);
#7109=AXIS2_PLACEMENT_3D('',#10827,#8572,#8573);
#7110=AXIS2_PLACEMENT_3D('',#10828,#8574,#8575);
#7111=AXIS2_PLACEMENT_3D('',#10829,#8576,#8577);
#7112=AXIS2_PLACEMENT_3D('',#10831,#8578,#8579);
#7113=AXIS2_PLACEMENT_3D('',#10833,#8580,#8581);
#7114=AXIS2_PLACEMENT_3D('',#10834,#8582,#8583);
#7115=AXIS2_PLACEMENT_3D('',#10835,#8584,#8585);
#7116=AXIS2_PLACEMENT_3D('',#10837,#8586,#8587);
#7117=AXIS2_PLACEMENT_3D('',#10839,#8588,#8589);
#7118=AXIS2_PLACEMENT_3D('',#10840,#8590,#8591);
#7119=AXIS2_PLACEMENT_3D('',#10841,#8592,#8593);
#7120=AXIS2_PLACEMENT_3D('',#10843,#8594,#8595);
#7121=AXIS2_PLACEMENT_3D('',#10845,#8596,#8597);
#7122=AXIS2_PLACEMENT_3D('',#10846,#8598,#8599);
#7123=AXIS2_PLACEMENT_3D('',#10847,#8600,#8601);
#7124=AXIS2_PLACEMENT_3D('',#10849,#8602,#8603);
#7125=AXIS2_PLACEMENT_3D('',#10851,#8604,#8605);
#7126=AXIS2_PLACEMENT_3D('',#10852,#8606,#8607);
#7127=AXIS2_PLACEMENT_3D('',#10853,#8608,#8609);
#7128=AXIS2_PLACEMENT_3D('',#10855,#8610,#8611);
#7129=AXIS2_PLACEMENT_3D('',#10857,#8612,#8613);
#7130=AXIS2_PLACEMENT_3D('',#10858,#8614,#8615);
#7131=AXIS2_PLACEMENT_3D('',#10860,#8616,#8617);
#7132=AXIS2_PLACEMENT_3D('',#10862,#8618,#8619);
#7133=AXIS2_PLACEMENT_3D('',#10863,#8620,#8621);
#7134=AXIS2_PLACEMENT_3D('',#10864,#8622,#8623);
#7135=AXIS2_PLACEMENT_3D('',#10866,#8624,#8625);
#7136=AXIS2_PLACEMENT_3D('',#10868,#8626,#8627);
#7137=AXIS2_PLACEMENT_3D('',#10869,#8628,#8629);
#7138=AXIS2_PLACEMENT_3D('',#10870,#8630,#8631);
#7139=AXIS2_PLACEMENT_3D('',#10872,#8632,#8633);
#7140=AXIS2_PLACEMENT_3D('',#10874,#8634,#8635);
#7141=AXIS2_PLACEMENT_3D('',#10875,#8636,#8637);
#7142=AXIS2_PLACEMENT_3D('',#10876,#8638,#8639);
#7143=AXIS2_PLACEMENT_3D('',#10878,#8640,#8641);
#7144=AXIS2_PLACEMENT_3D('',#10880,#8642,#8643);
#7145=AXIS2_PLACEMENT_3D('',#10881,#8644,#8645);
#7146=AXIS2_PLACEMENT_3D('',#10882,#8646,#8647);
#7147=AXIS2_PLACEMENT_3D('',#10884,#8648,#8649);
#7148=AXIS2_PLACEMENT_3D('',#10886,#8650,#8651);
#7149=AXIS2_PLACEMENT_3D('',#10887,#8652,#8653);
#7150=AXIS2_PLACEMENT_3D('',#10888,#8654,#8655);
#7151=AXIS2_PLACEMENT_3D('',#10890,#8656,#8657);
#7152=AXIS2_PLACEMENT_3D('',#10892,#8658,#8659);
#7153=AXIS2_PLACEMENT_3D('',#10893,#8660,#8661);
#7154=AXIS2_PLACEMENT_3D('',#10895,#8662,#8663);
#7155=AXIS2_PLACEMENT_3D('',#10897,#8664,#8665);
#7156=AXIS2_PLACEMENT_3D('',#10898,#8666,#8667);
#7157=AXIS2_PLACEMENT_3D('',#10900,#8668,#8669);
#7158=AXIS2_PLACEMENT_3D('',#10902,#8670,#8671);
#7159=AXIS2_PLACEMENT_3D('',#10904,#8672,#8673);
#7160=AXIS2_PLACEMENT_3D('',#10906,#8674,#8675);
#7161=AXIS2_PLACEMENT_3D('',#10908,#8676,#8677);
#7162=AXIS2_PLACEMENT_3D('',#10909,#8678,#8679);
#7163=AXIS2_PLACEMENT_3D('',#10911,#8680,#8681);
#7164=AXIS2_PLACEMENT_3D('',#10913,#8682,#8683);
#7165=AXIS2_PLACEMENT_3D('',#10915,#8684,#8685);
#7166=AXIS2_PLACEMENT_3D('',#10917,#8686,#8687);
#7167=AXIS2_PLACEMENT_3D('',#10918,#8688,#8689);
#7168=AXIS2_PLACEMENT_3D('',#10920,#8690,#8691);
#7169=AXIS2_PLACEMENT_3D('',#10922,#8692,#8693);
#7170=AXIS2_PLACEMENT_3D('',#10924,#8694,#8695);
#7171=AXIS2_PLACEMENT_3D('',#10926,#8696,#8697);
#7172=AXIS2_PLACEMENT_3D('',#10927,#8698,#8699);
#7173=AXIS2_PLACEMENT_3D('',#10929,#8700,#8701);
#7174=AXIS2_PLACEMENT_3D('',#10931,#8702,#8703);
#7175=AXIS2_PLACEMENT_3D('',#10933,#8704,#8705);
#7176=AXIS2_PLACEMENT_3D('',#10935,#8706,#8707);
#7177=AXIS2_PLACEMENT_3D('',#10936,#8708,#8709);
#7178=AXIS2_PLACEMENT_3D('',#10942,#8713,#8714);
#7179=AXIS2_PLACEMENT_3D('',#10944,#8715,#8716);
#7180=AXIS2_PLACEMENT_3D('',#10946,#8717,#8718);
#7181=AXIS2_PLACEMENT_3D('',#10948,#8719,#8720);
#7182=AXIS2_PLACEMENT_3D('',#10950,#8721,#8722);
#7183=AXIS2_PLACEMENT_3D('',#10952,#8723,#8724);
#7184=AXIS2_PLACEMENT_3D('',#10953,#8725,#8726);
#7185=AXIS2_PLACEMENT_3D('',#10955,#8727,#8728);
#7186=AXIS2_PLACEMENT_3D('',#10957,#8729,#8730);
#7187=AXIS2_PLACEMENT_3D('',#10959,#8731,#8732);
#7188=AXIS2_PLACEMENT_3D('',#10961,#8733,#8734);
#7189=AXIS2_PLACEMENT_3D('',#10962,#8735,#8736);
#7190=AXIS2_PLACEMENT_3D('',#10964,#8737,#8738);
#7191=AXIS2_PLACEMENT_3D('',#10966,#8739,#8740);
#7192=AXIS2_PLACEMENT_3D('',#10968,#8741,#8742);
#7193=AXIS2_PLACEMENT_3D('',#10970,#8743,#8744);
#7194=AXIS2_PLACEMENT_3D('',#10971,#8745,#8746);
#7195=AXIS2_PLACEMENT_3D('',#10973,#8747,#8748);
#7196=AXIS2_PLACEMENT_3D('',#10975,#8749,#8750);
#7197=AXIS2_PLACEMENT_3D('',#10977,#8751,#8752);
#7198=AXIS2_PLACEMENT_3D('',#10979,#8753,#8754);
#7199=AXIS2_PLACEMENT_3D('',#10981,#8755,#8756);
#7200=AXIS2_PLACEMENT_3D('',#10982,#8757,#8758);
#7201=AXIS2_PLACEMENT_3D('',#10984,#8759,#8760);
#7202=AXIS2_PLACEMENT_3D('',#10986,#8761,#8762);
#7203=AXIS2_PLACEMENT_3D('',#10987,#8763,#8764);
#7204=AXIS2_PLACEMENT_3D('',#10989,#8765,#8766);
#7205=AXIS2_PLACEMENT_3D('',#10991,#8767,#8768);
#7206=AXIS2_PLACEMENT_3D('',#10992,#8769,#8770);
#7207=AXIS2_PLACEMENT_3D('',#10993,#8771,#8772);
#7208=AXIS2_PLACEMENT_3D('',#10995,#8773,#8774);
#7209=AXIS2_PLACEMENT_3D('',#10997,#8775,#8776);
#7210=AXIS2_PLACEMENT_3D('',#10998,#8777,#8778);
#7211=AXIS2_PLACEMENT_3D('',#10999,#8779,#8780);
#7212=AXIS2_PLACEMENT_3D('',#11001,#8781,#8782);
#7213=AXIS2_PLACEMENT_3D('',#11003,#8783,#8784);
#7214=AXIS2_PLACEMENT_3D('',#11004,#8785,#8786);
#7215=AXIS2_PLACEMENT_3D('',#11005,#8787,#8788);
#7216=AXIS2_PLACEMENT_3D('',#11007,#8789,#8790);
#7217=AXIS2_PLACEMENT_3D('',#11009,#8791,#8792);
#7218=AXIS2_PLACEMENT_3D('',#11010,#8793,#8794);
#7219=AXIS2_PLACEMENT_3D('',#11011,#8795,#8796);
#7220=AXIS2_PLACEMENT_3D('',#11013,#8797,#8798);
#7221=AXIS2_PLACEMENT_3D('',#11015,#8799,#8800);
#7222=AXIS2_PLACEMENT_3D('',#11016,#8801,#8802);
#7223=AXIS2_PLACEMENT_3D('',#11017,#8803,#8804);
#7224=AXIS2_PLACEMENT_3D('',#11019,#8805,#8806);
#7225=AXIS2_PLACEMENT_3D('',#11021,#8807,#8808);
#7226=AXIS2_PLACEMENT_3D('',#11022,#8809,#8810);
#7227=AXIS2_PLACEMENT_3D('',#11024,#8811,#8812);
#7228=AXIS2_PLACEMENT_3D('',#11026,#8813,#8814);
#7229=AXIS2_PLACEMENT_3D('',#11027,#8815,#8816);
#7230=AXIS2_PLACEMENT_3D('',#11028,#8817,#8818);
#7231=AXIS2_PLACEMENT_3D('',#11030,#8819,#8820);
#7232=AXIS2_PLACEMENT_3D('',#11032,#8821,#8822);
#7233=AXIS2_PLACEMENT_3D('',#11033,#8823,#8824);
#7234=AXIS2_PLACEMENT_3D('',#11034,#8825,#8826);
#7235=AXIS2_PLACEMENT_3D('',#11036,#8827,#8828);
#7236=AXIS2_PLACEMENT_3D('',#11038,#8829,#8830);
#7237=AXIS2_PLACEMENT_3D('',#11039,#8831,#8832);
#7238=AXIS2_PLACEMENT_3D('',#11040,#8833,#8834);
#7239=AXIS2_PLACEMENT_3D('',#11042,#8835,#8836);
#7240=AXIS2_PLACEMENT_3D('',#11044,#8837,#8838);
#7241=AXIS2_PLACEMENT_3D('',#11045,#8839,#8840);
#7242=AXIS2_PLACEMENT_3D('',#11046,#8841,#8842);
#7243=AXIS2_PLACEMENT_3D('',#11048,#8843,#8844);
#7244=AXIS2_PLACEMENT_3D('',#11050,#8845,#8846);
#7245=AXIS2_PLACEMENT_3D('',#11051,#8847,#8848);
#7246=AXIS2_PLACEMENT_3D('',#11052,#8849,#8850);
#7247=AXIS2_PLACEMENT_3D('',#11054,#8851,#8852);
#7248=AXIS2_PLACEMENT_3D('',#11056,#8853,#8854);
#7249=AXIS2_PLACEMENT_3D('',#11057,#8855,#8856);
#7250=AXIS2_PLACEMENT_3D('',#11059,#8857,#8858);
#7251=AXIS2_PLACEMENT_3D('',#11061,#8859,#8860);
#7252=AXIS2_PLACEMENT_3D('',#11062,#8861,#8862);
#7253=AXIS2_PLACEMENT_3D('',#11064,#8863,#8864);
#7254=AXIS2_PLACEMENT_3D('',#11066,#8865,#8866);
#7255=AXIS2_PLACEMENT_3D('',#11068,#8867,#8868);
#7256=AXIS2_PLACEMENT_3D('',#11070,#8869,#8870);
#7257=AXIS2_PLACEMENT_3D('',#11071,#8871,#8872);
#7258=AXIS2_PLACEMENT_3D('',#11073,#8873,#8874);
#7259=AXIS2_PLACEMENT_3D('',#11075,#8875,#8876);
#7260=AXIS2_PLACEMENT_3D('',#11077,#8877,#8878);
#7261=AXIS2_PLACEMENT_3D('',#11079,#8879,#8880);
#7262=AXIS2_PLACEMENT_3D('',#11080,#8881,#8882);
#7263=AXIS2_PLACEMENT_3D('',#11082,#8883,#8884);
#7264=AXIS2_PLACEMENT_3D('',#11084,#8885,#8886);
#7265=AXIS2_PLACEMENT_3D('',#11086,#8887,#8888);
#7266=AXIS2_PLACEMENT_3D('',#11088,#8889,#8890);
#7267=AXIS2_PLACEMENT_3D('',#11089,#8891,#8892);
#7268=AXIS2_PLACEMENT_3D('',#11091,#8893,#8894);
#7269=AXIS2_PLACEMENT_3D('',#11093,#8895,#8896);
#7270=AXIS2_PLACEMENT_3D('',#11095,#8897,#8898);
#7271=AXIS2_PLACEMENT_3D('',#11097,#8899,#8900);
#7272=AXIS2_PLACEMENT_3D('',#11098,#8901,#8902);
#7273=AXIS2_PLACEMENT_3D('',#11100,#8903,#8904);
#7274=AXIS2_PLACEMENT_3D('',#11102,#8905,#8906);
#7275=AXIS2_PLACEMENT_3D('',#11104,#8907,#8908);
#7276=AXIS2_PLACEMENT_3D('',#11106,#8909,#8910);
#7277=AXIS2_PLACEMENT_3D('',#11107,#8911,#8912);
#7278=AXIS2_PLACEMENT_3D('',#11109,#8913,#8914);
#7279=AXIS2_PLACEMENT_3D('',#11111,#8915,#8916);
#7280=AXIS2_PLACEMENT_3D('',#11113,#8917,#8918);
#7281=AXIS2_PLACEMENT_3D('',#11115,#8919,#8920);
#7282=AXIS2_PLACEMENT_3D('',#11116,#8921,#8922);
#7283=AXIS2_PLACEMENT_3D('',#11118,#8923,#8924);
#7284=AXIS2_PLACEMENT_3D('',#11120,#8925,#8926);
#7285=AXIS2_PLACEMENT_3D('',#11122,#8927,#8928);
#7286=AXIS2_PLACEMENT_3D('',#11124,#8929,#8930);
#7287=AXIS2_PLACEMENT_3D('',#11125,#8931,#8932);
#7288=AXIS2_PLACEMENT_3D('',#11127,#8933,#8934);
#7289=AXIS2_PLACEMENT_3D('',#11129,#8935,#8936);
#7290=AXIS2_PLACEMENT_3D('',#11131,#8937,#8938);
#7291=AXIS2_PLACEMENT_3D('',#11133,#8939,#8940);
#7292=AXIS2_PLACEMENT_3D('',#11134,#8941,#8942);
#7293=AXIS2_PLACEMENT_3D('',#11136,#8943,#8944);
#7294=AXIS2_PLACEMENT_3D('',#11138,#8945,#8946);
#7295=AXIS2_PLACEMENT_3D('',#11140,#8947,#8948);
#7296=AXIS2_PLACEMENT_3D('',#11142,#8949,#8950);
#7297=AXIS2_PLACEMENT_3D('',#11143,#8951,#8952);
#7298=AXIS2_PLACEMENT_3D('',#11145,#8953,#8954);
#7299=AXIS2_PLACEMENT_3D('',#11147,#8955,#8956);
#7300=AXIS2_PLACEMENT_3D('',#11149,#8957,#8958);
#7301=AXIS2_PLACEMENT_3D('',#11151,#8959,#8960);
#7302=AXIS2_PLACEMENT_3D('',#11152,#8961,#8962);
#7303=AXIS2_PLACEMENT_3D('',#11154,#8963,#8964);
#7304=AXIS2_PLACEMENT_3D('',#11156,#8965,#8966);
#7305=AXIS2_PLACEMENT_3D('',#11158,#8967,#8968);
#7306=AXIS2_PLACEMENT_3D('',#11160,#8969,#8970);
#7307=AXIS2_PLACEMENT_3D('',#11161,#8971,#8972);
#7308=AXIS2_PLACEMENT_3D('',#11163,#8973,#8974);
#7309=AXIS2_PLACEMENT_3D('',#11165,#8975,#8976);
#7310=AXIS2_PLACEMENT_3D('',#11167,#8977,#8978);
#7311=AXIS2_PLACEMENT_3D('',#11168,#8979,#8980);
#7312=AXIS2_PLACEMENT_3D('',#11174,#8984,#8985);
#7313=AXIS2_PLACEMENT_3D('',#11176,#8987,#8988);
#7314=AXIS2_PLACEMENT_3D('',#11178,#8990,#8991);
#7315=AXIS2_PLACEMENT_3D('',#11180,#8993,#8994);
#7316=AXIS2_PLACEMENT_3D('',#11183,#8997,#8998);
#7317=AXIS2_PLACEMENT_3D('',#11184,#8999,#9000);
#7318=AXIS2_PLACEMENT_3D('',#11185,#9001,#9002);
#7319=AXIS2_PLACEMENT_3D('',#11187,#9004,#9005);
#7320=AXIS2_PLACEMENT_3D('',#11189,#9007,#9008);
#7321=AXIS2_PLACEMENT_3D('',#11191,#9010,#9011);
#7322=AXIS2_PLACEMENT_3D('',#11193,#9013,#9014);
#7323=AXIS2_PLACEMENT_3D('',#11194,#9015,#9016);
#7324=AXIS2_PLACEMENT_3D('',#11195,#9017,#9018);
#7325=AXIS2_PLACEMENT_3D('',#11197,#9020,#9021);
#7326=AXIS2_PLACEMENT_3D('',#11199,#9023,#9024);
#7327=AXIS2_PLACEMENT_3D('',#11200,#9025,#9026);
#7328=AXIS2_PLACEMENT_3D('',#11201,#9027,#9028);
#7329=AXIS2_PLACEMENT_3D('',#11203,#9030,#9031);
#7330=AXIS2_PLACEMENT_3D('',#11205,#9033,#9034);
#7331=AXIS2_PLACEMENT_3D('',#11206,#9035,#9036);
#7332=AXIS2_PLACEMENT_3D('',#11207,#9037,#9038);
#7333=AXIS2_PLACEMENT_3D('',#11209,#9040,#9041);
#7334=AXIS2_PLACEMENT_3D('',#11211,#9043,#9044);
#7335=AXIS2_PLACEMENT_3D('',#11212,#9045,#9046);
#7336=AXIS2_PLACEMENT_3D('',#11213,#9047,#9048);
#7337=AXIS2_PLACEMENT_3D('',#11215,#9050,#9051);
#7338=AXIS2_PLACEMENT_3D('',#11217,#9053,#9054);
#7339=AXIS2_PLACEMENT_3D('',#11218,#9055,#9056);
#7340=AXIS2_PLACEMENT_3D('',#11219,#9057,#9058);
#7341=AXIS2_PLACEMENT_3D('',#11221,#9060,#9061);
#7342=AXIS2_PLACEMENT_3D('',#11223,#9063,#9064);
#7343=AXIS2_PLACEMENT_3D('',#11224,#9065,#9066);
#7344=AXIS2_PLACEMENT_3D('',#11226,#9068,#9069);
#7345=AXIS2_PLACEMENT_3D('',#11227,#9070,#9071);
#7346=AXIS2_PLACEMENT_3D('',#11229,#9073,#9074);
#7347=AXIS2_PLACEMENT_3D('',#11230,#9075,#9076);
#7348=AXIS2_PLACEMENT_3D('',#11232,#9078,#9079);
#7349=AXIS2_PLACEMENT_3D('',#11233,#9080,#9081);
#7350=AXIS2_PLACEMENT_3D('',#11235,#9083,#9084);
#7351=AXIS2_PLACEMENT_3D('',#11236,#9085,#9086);
#7352=AXIS2_PLACEMENT_3D('',#11238,#9088,#9089);
#7353=AXIS2_PLACEMENT_3D('',#11239,#9090,#9091);
#7354=AXIS2_PLACEMENT_3D('',#11241,#9093,#9094);
#7355=AXIS2_PLACEMENT_3D('',#11242,#9095,#9096);
#7356=AXIS2_PLACEMENT_3D('',#11244,#9098,#9099);
#7357=AXIS2_PLACEMENT_3D('',#11245,#9100,#9101);
#7358=AXIS2_PLACEMENT_3D('',#11247,#9103,#9104);
#7359=AXIS2_PLACEMENT_3D('',#11248,#9105,#9106);
#7360=AXIS2_PLACEMENT_3D('',#11250,#9108,#9109);
#7361=AXIS2_PLACEMENT_3D('',#11251,#9110,#9111);
#7362=AXIS2_PLACEMENT_3D('',#11253,#9113,#9114);
#7363=AXIS2_PLACEMENT_3D('',#11254,#9115,#9116);
#7364=AXIS2_PLACEMENT_3D('',#11256,#9118,#9119);
#7365=AXIS2_PLACEMENT_3D('',#11258,#9121,#9122);
#7366=AXIS2_PLACEMENT_3D('',#11259,#9123,#9124);
#7367=AXIS2_PLACEMENT_3D('',#11261,#9126,#9127);
#7368=AXIS2_PLACEMENT_3D('',#11263,#9129,#9130);
#7369=AXIS2_PLACEMENT_3D('',#11264,#9131,#9132);
#7370=AXIS2_PLACEMENT_3D('',#11266,#9134,#9135);
#7371=AXIS2_PLACEMENT_3D('',#11268,#9137,#9138);
#7372=AXIS2_PLACEMENT_3D('',#11269,#9139,#9140);
#7373=AXIS2_PLACEMENT_3D('',#11271,#9142,#9143);
#7374=AXIS2_PLACEMENT_3D('',#11273,#9145,#9146);
#7375=AXIS2_PLACEMENT_3D('',#11274,#9147,#9148);
#7376=AXIS2_PLACEMENT_3D('',#11276,#9150,#9151);
#7377=AXIS2_PLACEMENT_3D('',#11278,#9153,#9154);
#7378=AXIS2_PLACEMENT_3D('',#11280,#9156,#9157);
#7379=AXIS2_PLACEMENT_3D('',#11282,#9159,#9160);
#7380=AXIS2_PLACEMENT_3D('',#11283,#9161,#9162);
#7381=AXIS2_PLACEMENT_3D('',#11285,#9164,#9165);
#7382=AXIS2_PLACEMENT_3D('',#11287,#9167,#9168);
#7383=AXIS2_PLACEMENT_3D('',#11289,#9170,#9171);
#7384=AXIS2_PLACEMENT_3D('',#11291,#9173,#9174);
#7385=AXIS2_PLACEMENT_3D('',#11292,#9175,#9176);
#7386=AXIS2_PLACEMENT_3D('',#11294,#9178,#9179);
#7387=AXIS2_PLACEMENT_3D('',#11296,#9181,#9182);
#7388=AXIS2_PLACEMENT_3D('',#11298,#9184,#9185);
#7389=AXIS2_PLACEMENT_3D('',#11300,#9187,#9188);
#7390=AXIS2_PLACEMENT_3D('',#11301,#9189,#9190);
#7391=AXIS2_PLACEMENT_3D('',#11303,#9192,#9193);
#7392=AXIS2_PLACEMENT_3D('',#11305,#9195,#9196);
#7393=AXIS2_PLACEMENT_3D('',#11307,#9198,#9199);
#7394=AXIS2_PLACEMENT_3D('',#11309,#9201,#9202);
#7395=AXIS2_PLACEMENT_3D('',#11310,#9203,#9204);
#7396=AXIS2_PLACEMENT_3D('',#11312,#9206,#9207);
#7397=AXIS2_PLACEMENT_3D('',#11314,#9209,#9210);
#7398=AXIS2_PLACEMENT_3D('',#11316,#9212,#9213);
#7399=AXIS2_PLACEMENT_3D('',#11318,#9215,#9216);
#7400=AXIS2_PLACEMENT_3D('',#11319,#9217,#9218);
#7401=AXIS2_PLACEMENT_3D('',#11321,#9220,#9221);
#7402=AXIS2_PLACEMENT_3D('',#11323,#9223,#9224);
#7403=AXIS2_PLACEMENT_3D('',#11325,#9226,#9227);
#7404=AXIS2_PLACEMENT_3D('',#11327,#9229,#9230);
#7405=AXIS2_PLACEMENT_3D('',#11328,#9231,#9232);
#7406=AXIS2_PLACEMENT_3D('',#11330,#9234,#9235);
#7407=AXIS2_PLACEMENT_3D('',#11332,#9237,#9238);
#7408=AXIS2_PLACEMENT_3D('',#11334,#9240,#9241);
#7409=AXIS2_PLACEMENT_3D('',#11336,#9243,#9244);
#7410=AXIS2_PLACEMENT_3D('',#11337,#9245,#9246);
#7411=AXIS2_PLACEMENT_3D('',#11339,#9248,#9249);
#7412=AXIS2_PLACEMENT_3D('',#11341,#9251,#9252);
#7413=AXIS2_PLACEMENT_3D('',#11343,#9254,#9255);
#7414=AXIS2_PLACEMENT_3D('',#11345,#9257,#9258);
#7415=AXIS2_PLACEMENT_3D('',#11346,#9259,#9260);
#7416=AXIS2_PLACEMENT_3D('',#11348,#9262,#9263);
#7417=AXIS2_PLACEMENT_3D('',#11350,#9265,#9266);
#7418=AXIS2_PLACEMENT_3D('',#11352,#9268,#9269);
#7419=AXIS2_PLACEMENT_3D('',#11354,#9271,#9272);
#7420=AXIS2_PLACEMENT_3D('',#11355,#9273,#9274);
#7421=AXIS2_PLACEMENT_3D('',#11357,#9276,#9277);
#7422=AXIS2_PLACEMENT_3D('',#11359,#9279,#9280);
#7423=AXIS2_PLACEMENT_3D('',#11361,#9282,#9283);
#7424=AXIS2_PLACEMENT_3D('',#11363,#9285,#9286);
#7425=AXIS2_PLACEMENT_3D('',#11364,#9287,#9288);
#7426=AXIS2_PLACEMENT_3D('',#11366,#9290,#9291);
#7427=AXIS2_PLACEMENT_3D('',#11368,#9293,#9294);
#7428=AXIS2_PLACEMENT_3D('',#11370,#9296,#9297);
#7429=AXIS2_PLACEMENT_3D('',#11372,#9299,#9300);
#7430=AXIS2_PLACEMENT_3D('',#11373,#9301,#9302);
#7431=AXIS2_PLACEMENT_3D('',#11375,#9304,#9305);
#7432=AXIS2_PLACEMENT_3D('',#11377,#9307,#9308);
#7433=AXIS2_PLACEMENT_3D('',#11379,#9310,#9311);
#7434=AXIS2_PLACEMENT_3D('',#11381,#9313,#9314);
#7435=AXIS2_PLACEMENT_3D('',#11382,#9315,#9316);
#7436=AXIS2_PLACEMENT_3D('',#11384,#9318,#9319);
#7437=AXIS2_PLACEMENT_3D('',#11386,#9321,#9322);
#7438=AXIS2_PLACEMENT_3D('',#11388,#9324,#9325);
#7439=AXIS2_PLACEMENT_3D('',#11390,#9327,#9328);
#7440=AXIS2_PLACEMENT_3D('',#11391,#9329,#9330);
#7441=AXIS2_PLACEMENT_3D('',#11393,#9332,#9333);
#7442=AXIS2_PLACEMENT_3D('',#11395,#9335,#9336);
#7443=AXIS2_PLACEMENT_3D('',#11397,#9338,#9339);
#7444=AXIS2_PLACEMENT_3D('',#11399,#9341,#9342);
#7445=AXIS2_PLACEMENT_3D('',#11400,#9343,#9344);
#7446=AXIS2_PLACEMENT_3D('',#11402,#9346,#9347);
#7447=AXIS2_PLACEMENT_3D('',#11404,#9349,#9350);
#7448=AXIS2_PLACEMENT_3D('',#11405,#9351,#9352);
#7449=AXIS2_PLACEMENT_3D('',#11406,#9353,#9354);
#7450=AXIS2_PLACEMENT_3D('',#11408,#9355,#9356);
#7451=AXIS2_PLACEMENT_3D('',#11411,#9358,#9359);
#7452=AXIS2_PLACEMENT_3D('',#11412,#9360,#9361);
#7453=AXIS2_PLACEMENT_3D('',#11415,#9362,#9363);
#7454=AXIS2_PLACEMENT_3D('',#11419,#9365,#9366);
#7455=AXIS2_PLACEMENT_3D('',#11423,#9368,#9369);
#7456=AXIS2_PLACEMENT_3D('',#11427,#9371,#9372);
#7457=AXIS2_PLACEMENT_3D('',#11429,#9374,#9375);
#7458=AXIS2_PLACEMENT_3D('',#11431,#9376,#9377);
#7459=AXIS2_PLACEMENT_3D('',#11434,#9379,#9380);
#7460=AXIS2_PLACEMENT_3D('',#11435,#9381,#9382);
#7461=AXIS2_PLACEMENT_3D('',#11449,#9389,#9390);
#7462=AXIS2_PLACEMENT_3D('',#11451,#9391,#9392);
#7463=AXIS2_PLACEMENT_3D('',#11455,#9395,#9396);
#7464=AXIS2_PLACEMENT_3D('',#11465,#9402,#9403);
#7465=AXIS2_PLACEMENT_3D('',#11476,#9408,#9409);
#7466=AXIS2_PLACEMENT_3D('',#11478,#9410,#9411);
#7467=AXIS2_PLACEMENT_3D('',#11485,#9416,#9417);
#7468=AXIS2_PLACEMENT_3D('',#11495,#9423,#9424);
#7469=AXIS2_PLACEMENT_3D('',#11497,#9426,#9427);
#7470=AXIS2_PLACEMENT_3D('',#11499,#9429,#9430);
#7471=AXIS2_PLACEMENT_3D('',#11501,#9432,#9433);
#7472=AXIS2_PLACEMENT_3D('',#11503,#9435,#9436);
#7473=AXIS2_PLACEMENT_3D('',#11505,#9438,#9439);
#7474=AXIS2_PLACEMENT_3D('',#11508,#9442,#9443);
#7475=AXIS2_PLACEMENT_3D('',#11510,#9445,#9446);
#7476=AXIS2_PLACEMENT_3D('',#11520,#9452,#9453);
#7477=AXIS2_PLACEMENT_3D('',#11526,#9457,#9458);
#7478=AXIS2_PLACEMENT_3D('',#11536,#9466,#9467);
#7479=AXIS2_PLACEMENT_3D('',#11537,#9468,#9469);
#7480=AXIS2_PLACEMENT_3D('',#11538,#9470,#9471);
#7481=AXIS2_PLACEMENT_3D('',#11539,#9472,#9473);
#7482=AXIS2_PLACEMENT_3D('',#11541,#9475,#9476);
#7483=AXIS2_PLACEMENT_3D('',#11542,#9477,#9478);
#7484=AXIS2_PLACEMENT_3D('',#11544,#9480,#9481);
#7485=AXIS2_PLACEMENT_3D('',#11545,#9482,#9483);
#7486=AXIS2_PLACEMENT_3D('',#11546,#9484,#9485);
#7487=AXIS2_PLACEMENT_3D('',#11547,#9486,#9487);
#7488=AXIS2_PLACEMENT_3D('',#11549,#9488,#9489);
#7489=AXIS2_PLACEMENT_3D('',#11553,#9491,#9492);
#7490=AXIS2_PLACEMENT_3D('',#11557,#9494,#9495);
#7491=AXIS2_PLACEMENT_3D('',#11561,#9497,#9498);
#7492=AXIS2_PLACEMENT_3D('',#11565,#9500,#9501);
#7493=AXIS2_PLACEMENT_3D('',#11568,#9503,#9504);
#7494=AXIS2_PLACEMENT_3D('',#11569,#9505,#9506);
#7495=AXIS2_PLACEMENT_3D('',#11571,#9507,#9508);
#7496=AXIS2_PLACEMENT_3D('',#11574,#9510,#9511);
#7497=AXIS2_PLACEMENT_3D('',#11575,#9512,#9513);
#7498=AXIS2_PLACEMENT_3D('',#11579,#9515,#9516);
#7499=AXIS2_PLACEMENT_3D('',#11581,#9518,#9519);
#7500=AXIS2_PLACEMENT_3D('',#11585,#9521,#9522);
#7501=AXIS2_PLACEMENT_3D('',#11587,#9524,#9525);
#7502=AXIS2_PLACEMENT_3D('',#11588,#9526,#9527);
#7503=AXIS2_PLACEMENT_3D('',#11591,#9528,#9529);
#7504=AXIS2_PLACEMENT_3D('',#11595,#9531,#9532);
#7505=AXIS2_PLACEMENT_3D('',#11597,#9534,#9535);
#7506=AXIS2_PLACEMENT_3D('',#11600,#9536,#9537);
#7507=AXIS2_PLACEMENT_3D('',#11603,#9540,#9541);
#7508=AXIS2_PLACEMENT_3D('',#11607,#9544,#9545);
#7509=AXIS2_PLACEMENT_3D('',#11609,#9546,#9547);
#7510=AXIS2_PLACEMENT_3D('',#11611,#9549,#9550);
#7511=AXIS2_PLACEMENT_3D('',#11613,#9552,#9553);
#7512=AXIS2_PLACEMENT_3D('',#11614,#9554,#9555);
#7513=AXIS2_PLACEMENT_3D('',#11617,#9556,#9557);
#7514=AXIS2_PLACEMENT_3D('',#11620,#9560,#9561);
#7515=AXIS2_PLACEMENT_3D('',#11623,#9562,#9563);
#7516=AXIS2_PLACEMENT_3D('',#11626,#9566,#9567);
#7517=AXIS2_PLACEMENT_3D('',#11631,#9572,#9573);
#7518=AXIS2_PLACEMENT_3D('',#11632,#9574,#9575);
#7519=AXIS2_PLACEMENT_3D('',#11633,#9576,#9577);
#7520=AXIS2_PLACEMENT_3D('',#11634,#9578,#9579);
#7521=AXIS2_PLACEMENT_3D('',#11635,#9580,#9581);
#7522=AXIS2_PLACEMENT_3D('',#11636,#9582,#9583);
#7523=AXIS2_PLACEMENT_3D('',#11639,#9584,#9585);
#7524=AXIS2_PLACEMENT_3D('',#11643,#9587,#9588);
#7525=AXIS2_PLACEMENT_3D('',#11645,#9590,#9591);
#7526=AXIS2_PLACEMENT_3D('',#11648,#9592,#9593);
#7527=AXIS2_PLACEMENT_3D('',#11652,#9595,#9596);
#7528=AXIS2_PLACEMENT_3D('',#11654,#9598,#9599);
#7529=AXIS2_PLACEMENT_3D('',#11656,#9600,#9601);
#7530=AXIS2_PLACEMENT_3D('',#11659,#9603,#9604);
#7531=AXIS2_PLACEMENT_3D('',#11660,#9605,#9606);
#7532=AXIS2_PLACEMENT_3D('',#11662,#9607,#9608);
#7533=AXIS2_PLACEMENT_3D('',#11665,#9610,#9611);
#7534=AXIS2_PLACEMENT_3D('',#11666,#9612,#9613);
#7535=AXIS2_PLACEMENT_3D('',#11669,#9614,#9615);
#7536=AXIS2_PLACEMENT_3D('',#11673,#9617,#9618);
#7537=AXIS2_PLACEMENT_3D('',#11675,#9620,#9621);
#7538=AXIS2_PLACEMENT_3D('',#11679,#9623,#9624);
#7539=AXIS2_PLACEMENT_3D('',#11683,#9626,#9627);
#7540=AXIS2_PLACEMENT_3D('',#11686,#9630,#9631);
#7541=AXIS2_PLACEMENT_3D('',#11690,#9634,#9635);
#7542=AXIS2_PLACEMENT_3D('',#11694,#9638,#9639);
#7543=AXIS2_PLACEMENT_3D('',#11695,#9640,#9641);
#7544=AXIS2_PLACEMENT_3D('',#11696,#9642,#9643);
#7545=AXIS2_PLACEMENT_3D('',#11700,#9645,#9646);
#7546=AXIS2_PLACEMENT_3D('',#11702,#9648,#9649);
#7547=AXIS2_PLACEMENT_3D('',#11706,#9652,#9653);
#7548=AXIS2_PLACEMENT_3D('',#11708,#9654,#9655);
#7549=AXIS2_PLACEMENT_3D('',#11710,#9657,#9658);
#7550=AXIS2_PLACEMENT_3D('',#11712,#9660,#9661);
#7551=AXIS2_PLACEMENT_3D('',#11713,#9662,#9663);
#7552=AXIS2_PLACEMENT_3D('',#11717,#9665,#9666);
#7553=AXIS2_PLACEMENT_3D('',#11719,#9668,#9669);
#7554=AXIS2_PLACEMENT_3D('',#11721,#9671,#9672);
#7555=AXIS2_PLACEMENT_3D('',#11723,#9674,#9675);
#7556=AXIS2_PLACEMENT_3D('',#11724,#9676,#9677);
#7557=AXIS2_PLACEMENT_3D('',#11725,#9678,#9679);
#7558=AXIS2_PLACEMENT_3D('',#11727,#9680,#9681);
#7559=AXIS2_PLACEMENT_3D('',#11731,#9683,#9684);
#7560=AXIS2_PLACEMENT_3D('',#11735,#9686,#9687);
#7561=AXIS2_PLACEMENT_3D('',#11739,#9689,#9690);
#7562=AXIS2_PLACEMENT_3D('',#11743,#9692,#9693);
#7563=AXIS2_PLACEMENT_3D('',#11746,#9695,#9696);
#7564=AXIS2_PLACEMENT_3D('',#11747,#9697,#9698);
#7565=AXIS2_PLACEMENT_3D('',#11749,#9699,#9700);
#7566=AXIS2_PLACEMENT_3D('',#11752,#9702,#9703);
#7567=AXIS2_PLACEMENT_3D('',#11753,#9704,#9705);
#7568=AXIS2_PLACEMENT_3D('',#11757,#9707,#9708);
#7569=AXIS2_PLACEMENT_3D('',#11759,#9710,#9711);
#7570=AXIS2_PLACEMENT_3D('',#11763,#9713,#9714);
#7571=AXIS2_PLACEMENT_3D('',#11765,#9716,#9717);
#7572=AXIS2_PLACEMENT_3D('',#11766,#9718,#9719);
#7573=AXIS2_PLACEMENT_3D('',#11769,#9720,#9721);
#7574=AXIS2_PLACEMENT_3D('',#11772,#9724,#9725);
#7575=AXIS2_PLACEMENT_3D('',#11775,#9726,#9727);
#7576=AXIS2_PLACEMENT_3D('',#11778,#9730,#9731);
#7577=AXIS2_PLACEMENT_3D('',#11783,#9736,#9737);
#7578=AXIS2_PLACEMENT_3D('',#11784,#9738,#9739);
#7579=AXIS2_PLACEMENT_3D('',#11785,#9740,#9741);
#7580=AXIS2_PLACEMENT_3D('',#11786,#9742,#9743);
#7581=AXIS2_PLACEMENT_3D('',#11787,#9744,#9745);
#7582=AXIS2_PLACEMENT_3D('',#11790,#9746,#9747);
#7583=AXIS2_PLACEMENT_3D('',#11794,#9749,#9750);
#7584=AXIS2_PLACEMENT_3D('',#11796,#9752,#9753);
#7585=AXIS2_PLACEMENT_3D('',#11800,#9755,#9756);
#7586=AXIS2_PLACEMENT_3D('',#11802,#9758,#9759);
#7587=AXIS2_PLACEMENT_3D('',#11806,#9762,#9763);
#7588=AXIS2_PLACEMENT_3D('',#11809,#9765,#9766);
#7589=AXIS2_PLACEMENT_3D('',#11810,#9767,#9768);
#7590=AXIS2_PLACEMENT_3D('',#11812,#9770,#9771);
#7591=AXIS2_PLACEMENT_3D('',#11813,#9772,#9773);
#7592=AXIS2_PLACEMENT_3D('',#11814,#9774,#9775);
#7593=AXIS2_PLACEMENT_3D('',#11817,#9776,#9777);
#7594=AXIS2_PLACEMENT_3D('',#11818,#9778,#9779);
#7595=AXIS2_PLACEMENT_3D('',#11820,#9780,#9781);
#7596=AXIS2_PLACEMENT_3D('',#11821,#9782,#9783);
#7597=AXIS2_PLACEMENT_3D('',#11822,#9784,#9785);
#7598=AXIS2_PLACEMENT_3D('',#11825,#9786,#9787);
#7599=AXIS2_PLACEMENT_3D('',#11829,#9789,#9790);
#7600=AXIS2_PLACEMENT_3D('',#11831,#9792,#9793);
#7601=AXIS2_PLACEMENT_3D('',#11834,#9795,#9796);
#7602=AXIS2_PLACEMENT_3D('',#11835,#9797,#9798);
#7603=AXIS2_PLACEMENT_3D('',#11838,#9799,#9800);
#7604=AXIS2_PLACEMENT_3D('',#11842,#9802,#9803);
#7605=AXIS2_PLACEMENT_3D('',#11845,#9805,#9806);
#7606=AXIS2_PLACEMENT_3D('',#11847,#9807,#9808);
#7607=AXIS2_PLACEMENT_3D('',#11851,#9810,#9811);
#7608=AXIS2_PLACEMENT_3D('',#11855,#9813,#9814);
#7609=AXIS2_PLACEMENT_3D('',#11857,#9816,#9817);
#7610=AXIS2_PLACEMENT_3D('',#11861,#9819,#9820);
#7611=AXIS2_PLACEMENT_3D('',#11863,#9822,#9823);
#7612=AXIS2_PLACEMENT_3D('',#11866,#9826,#9827);
#7613=AXIS2_PLACEMENT_3D('',#11870,#9829,#9830);
#7614=AXIS2_PLACEMENT_3D('',#11874,#9834,#9835);
#7615=AXIS2_PLACEMENT_3D('',#11877,#9838,#9839);
#7616=AXIS2_PLACEMENT_3D('',#11878,#9840,#9841);
#7617=AXIS2_PLACEMENT_3D('',#11879,#9842,#9843);
#7618=AXIS2_PLACEMENT_3D('',#11880,#9844,#9845);
#7619=AXIS2_PLACEMENT_3D('',#11881,#9846,#9847);
#7620=AXIS2_PLACEMENT_3D('',#11882,#9848,#9849);
#7621=AXIS2_PLACEMENT_3D('',#11883,#9850,#9851);
#7622=AXIS2_PLACEMENT_3D('',#11884,#9852,#9853);
#7623=AXIS2_PLACEMENT_3D('',#11885,#9854,#9855);
#7624=AXIS2_PLACEMENT_3D('',#11886,#9856,#9857);
#7625=AXIS2_PLACEMENT_3D('',#11887,#9858,#9859);
#7626=AXIS2_PLACEMENT_3D('',#11888,#9860,#9861);
#7627=AXIS2_PLACEMENT_3D('',#11889,#9862,#9863);
#7628=AXIS2_PLACEMENT_3D('',#11890,#9864,#9865);
#7629=AXIS2_PLACEMENT_3D('',#11891,#9866,#9867);
#7630=AXIS2_PLACEMENT_3D('',#11892,#9868,#9869);
#7631=AXIS2_PLACEMENT_3D('',#11893,#9870,#9871);
#7632=AXIS2_PLACEMENT_3D('',#11894,#9872,#9873);
#7633=AXIS2_PLACEMENT_3D('',#11895,#9874,#9875);
#7634=AXIS2_PLACEMENT_3D('',#11896,#9876,#9877);
#7635=AXIS2_PLACEMENT_3D('',#11897,#9878,#9879);
#7636=AXIS2_PLACEMENT_3D('',#11898,#9880,#9881);
#7637=AXIS2_PLACEMENT_3D('',#11899,#9882,#9883);
#7638=AXIS2_PLACEMENT_3D('',#11900,#9884,#9885);
#7639=AXIS2_PLACEMENT_3D('',#11901,#9886,#9887);
#7640=AXIS2_PLACEMENT_3D('',#11902,#9888,#9889);
#7641=AXIS2_PLACEMENT_3D('',#11903,#9890,#9891);
#7642=AXIS2_PLACEMENT_3D('',#11904,#9892,#9893);
#7643=AXIS2_PLACEMENT_3D('',#11905,#9894,#9895);
#7644=AXIS2_PLACEMENT_3D('',#11906,#9896,#9897);
#7645=AXIS2_PLACEMENT_3D('',#11907,#9898,#9899);
#7646=AXIS2_PLACEMENT_3D('',#11908,#9900,#9901);
#7647=AXIS2_PLACEMENT_3D('',#11909,#9902,#9903);
#7648=AXIS2_PLACEMENT_3D('',#11910,#9904,#9905);
#7649=AXIS2_PLACEMENT_3D('',#11911,#9906,#9907);
#7650=DIRECTION('axis',(0.,0.,1.));
#7651=DIRECTION('refdir',(1.,0.,0.));
#7652=DIRECTION('axis',(0.,0.,1.));
#7653=DIRECTION('refdir',(1.,0.,0.));
#7654=DIRECTION('center_axis',(0.,0.,-1.));
#7655=DIRECTION('ref_axis',(-1.,0.,0.));
#7656=DIRECTION('center_axis',(0.,0.,-1.));
#7657=DIRECTION('ref_axis',(1.,0.,0.));
#7658=DIRECTION('',(0.,0.,-1.));
#7659=DIRECTION('center_axis',(0.,0.,-1.));
#7660=DIRECTION('ref_axis',(1.,0.,0.));
#7661=DIRECTION('center_axis',(0.,0.,-1.));
#7662=DIRECTION('ref_axis',(-1.,0.,0.));
#7663=DIRECTION('center_axis',(0.,0.,1.));
#7664=DIRECTION('ref_axis',(1.,0.,0.));
#7665=DIRECTION('',(0.,0.,-1.));
#7666=DIRECTION('center_axis',(0.,0.,1.));
#7667=DIRECTION('ref_axis',(1.,0.,0.));
#7668=DIRECTION('center_axis',(0.,0.,-1.));
#7669=DIRECTION('ref_axis',(-1.,0.,0.));
#7670=DIRECTION('center_axis',(0.,0.,1.));
#7671=DIRECTION('ref_axis',(1.,0.,0.));
#7672=DIRECTION('',(0.,0.,-1.));
#7673=DIRECTION('center_axis',(0.,0.,1.));
#7674=DIRECTION('ref_axis',(1.,0.,0.));
#7675=DIRECTION('center_axis',(0.,0.,-1.));
#7676=DIRECTION('ref_axis',(-1.,0.,0.));
#7677=DIRECTION('center_axis',(0.,0.,1.));
#7678=DIRECTION('ref_axis',(1.,0.,0.));
#7679=DIRECTION('',(0.,0.,-1.));
#7680=DIRECTION('center_axis',(0.,0.,1.));
#7681=DIRECTION('ref_axis',(1.,0.,0.));
#7682=DIRECTION('center_axis',(0.707106781186548,0.707106781186548,0.));
#7683=DIRECTION('ref_axis',(-0.707106781186548,0.707106781186548,0.));
#7684=DIRECTION('',(0.707106781186547,-0.707106781186547,0.));
#7685=DIRECTION('',(0.,0.,-1.));
#7686=DIRECTION('',(0.707106781186547,-0.707106781186547,0.));
#7687=DIRECTION('',(0.,0.,-1.));
#7688=DIRECTION('center_axis',(0.,1.,0.));
#7689=DIRECTION('ref_axis',(0.,0.,1.));
#7690=DIRECTION('',(1.,0.,0.));
#7691=DIRECTION('',(0.,0.,-1.));
#7692=DIRECTION('',(1.,0.,0.));
#7693=DIRECTION('center_axis',(0.707106781186548,-0.707106781186548,0.));
#7694=DIRECTION('ref_axis',(0.707106781186548,0.707106781186548,0.));
#7695=DIRECTION('',(-0.707106781186547,-0.707106781186547,0.));
#7696=DIRECTION('',(0.,0.,-1.));
#7697=DIRECTION('',(-0.707106781186547,-0.707106781186547,0.));
#7698=DIRECTION('center_axis',(-1.,2.56996070515082E-16,0.));
#7699=DIRECTION('ref_axis',(-2.56996070515082E-16,-1.,0.));
#7700=DIRECTION('',(2.56996070515082E-16,1.,0.));
#7701=DIRECTION('',(0.,0.,1.));
#7702=DIRECTION('',(2.56996070515082E-16,1.,0.));
#7703=DIRECTION('center_axis',(0.,-1.,0.));
#7704=DIRECTION('ref_axis',(0.,0.,-1.));
#7705=DIRECTION('',(-1.,0.,0.));
#7706=DIRECTION('',(0.,0.,-1.));
#7707=DIRECTION('',(-1.,0.,0.));
#7708=DIRECTION('',(0.,0.,1.));
#7709=DIRECTION('center_axis',(0.,0.,-1.));
#7710=DIRECTION('ref_axis',(-1.,0.,0.));
#7711=DIRECTION('center_axis',(0.,0.,1.));
#7712=DIRECTION('ref_axis',(1.,0.,0.));
#7713=DIRECTION('',(0.,0.,-1.));
#7714=DIRECTION('center_axis',(0.,0.,1.));
#7715=DIRECTION('ref_axis',(1.,0.,0.));
#7716=DIRECTION('',(0.,0.,-1.));
#7717=DIRECTION('center_axis',(0.,0.,-1.));
#7718=DIRECTION('ref_axis',(-1.,0.,0.));
#7719=DIRECTION('center_axis',(0.,0.,-1.));
#7720=DIRECTION('ref_axis',(1.,1.77635683940025E-15,0.));
#7721=DIRECTION('',(0.,0.,-1.));
#7722=DIRECTION('center_axis',(0.,0.,-1.));
#7723=DIRECTION('ref_axis',(1.,1.77635683940025E-15,0.));
#7724=DIRECTION('center_axis',(0.,1.,0.));
#7725=DIRECTION('ref_axis',(0.,0.,1.));
#7726=DIRECTION('',(1.,0.,0.));
#7727=DIRECTION('',(0.,0.,-1.));
#7728=DIRECTION('',(1.,0.,0.));
#7729=DIRECTION('center_axis',(0.,0.,-1.));
#7730=DIRECTION('ref_axis',(-1.,0.,0.));
#7731=DIRECTION('center_axis',(0.,0.,-1.));
#7732=DIRECTION('ref_axis',(1.,8.88178419700125E-16,0.));
#7733=DIRECTION('',(0.,0.,-1.));
#7734=DIRECTION('center_axis',(0.,0.,-1.));
#7735=DIRECTION('ref_axis',(1.,8.88178419700125E-16,0.));
#7736=DIRECTION('',(0.,0.,-1.));
#7737=DIRECTION('center_axis',(0.,0.,-1.));
#7738=DIRECTION('ref_axis',(-1.,0.,0.));
#7739=DIRECTION('center_axis',(0.,0.,1.));
#7740=DIRECTION('ref_axis',(1.,0.,0.));
#7741=DIRECTION('',(0.,0.,-1.));
#7742=DIRECTION('center_axis',(0.,0.,1.));
#7743=DIRECTION('ref_axis',(1.,0.,0.));
#7744=DIRECTION('center_axis',(0.,0.,-1.));
#7745=DIRECTION('ref_axis',(-1.,0.,0.));
#7746=DIRECTION('center_axis',(0.,0.,1.));
#7747=DIRECTION('ref_axis',(1.,0.,0.));
#7748=DIRECTION('',(0.,0.,-1.));
#7749=DIRECTION('center_axis',(0.,0.,1.));
#7750=DIRECTION('ref_axis',(1.,0.,0.));
#7751=DIRECTION('center_axis',(1.,1.28498035257541E-16,0.));
#7752=DIRECTION('ref_axis',(-1.28498035257541E-16,1.,0.));
#7753=DIRECTION('',(1.28498035257541E-16,-1.,0.));
#7754=DIRECTION('',(0.,0.,-1.));
#7755=DIRECTION('',(1.28498035257541E-16,-1.,0.));
#7756=DIRECTION('center_axis',(0.,0.,-1.));
#7757=DIRECTION('ref_axis',(-1.,0.,0.));
#7758=DIRECTION('center_axis',(0.,0.,1.));
#7759=DIRECTION('ref_axis',(1.,0.,0.));
#7760=DIRECTION('center_axis',(0.,0.,1.));
#7761=DIRECTION('ref_axis',(1.,0.,0.));
#7762=DIRECTION('center_axis',(0.,1.,0.));
#7763=DIRECTION('ref_axis',(0.,0.,1.));
#7764=DIRECTION('',(1.,0.,0.));
#7765=DIRECTION('',(1.,0.,0.));
#7766=DIRECTION('center_axis',(0.,0.,1.));
#7767=DIRECTION('ref_axis',(1.,0.,0.));
#7768=DIRECTION('center_axis',(0.,0.,1.));
#7769=DIRECTION('ref_axis',(1.,0.,0.));
#7770=DIRECTION('center_axis',(0.,0.,1.));
#7771=DIRECTION('ref_axis',(1.,0.,0.));
#7772=DIRECTION('center_axis',(0.,0.,1.));
#7773=DIRECTION('ref_axis',(1.,0.,0.));
#7774=DIRECTION('center_axis',(0.,0.,-1.));
#7775=DIRECTION('ref_axis',(1.,0.,0.));
#7776=DIRECTION('center_axis',(0.,0.,-1.));
#7777=DIRECTION('ref_axis',(1.,0.,0.));
#7778=DIRECTION('center_axis',(0.,0.,-1.));
#7779=DIRECTION('ref_axis',(-1.,0.,0.));
#7780=DIRECTION('center_axis',(0.,0.,-1.));
#7781=DIRECTION('ref_axis',(-1.,0.,0.));
#7782=DIRECTION('axis',(0.,0.,1.));
#7783=DIRECTION('refdir',(1.,0.,0.));
#7784=DIRECTION('center_axis',(0.,0.,-1.));
#7785=DIRECTION('ref_axis',(-1.,0.,0.));
#7786=DIRECTION('center_axis',(0.,0.,1.));
#7787=DIRECTION('ref_axis',(1.,0.,0.));
#7788=DIRECTION('',(0.,0.,1.));
#7789=DIRECTION('center_axis',(0.,0.,1.));
#7790=DIRECTION('ref_axis',(1.,0.,0.));
#7791=DIRECTION('center_axis',(0.,0.,-1.));
#7792=DIRECTION('ref_axis',(-1.,0.,0.));
#7793=DIRECTION('center_axis',(0.,0.,-1.));
#7794=DIRECTION('ref_axis',(1.,0.,0.));
#7795=DIRECTION('',(0.,0.,-1.));
#7796=DIRECTION('center_axis',(0.,0.,-1.));
#7797=DIRECTION('ref_axis',(1.,0.,0.));
#7798=DIRECTION('',(0.,0.,-1.));
#7799=DIRECTION('center_axis',(0.,0.,1.));
#7800=DIRECTION('ref_axis',(1.,0.,0.));
#7801=DIRECTION('center_axis',(0.,0.,-1.));
#7802=DIRECTION('ref_axis',(1.,0.,0.));
#7803=DIRECTION('',(0.,0.,1.));
#7804=DIRECTION('center_axis',(0.,0.,-1.));
#7805=DIRECTION('ref_axis',(1.,0.,0.));
#7806=DIRECTION('',(0.,0.,1.));
#7807=DIRECTION('center_axis',(0.,0.,-1.));
#7808=DIRECTION('ref_axis',(-1.,0.,0.));
#7809=DIRECTION('center_axis',(0.,0.,-1.));
#7810=DIRECTION('ref_axis',(1.,0.,0.));
#7811=DIRECTION('',(0.,0.,-1.));
#7812=DIRECTION('center_axis',(0.,0.,1.));
#7813=DIRECTION('ref_axis',(1.,0.,0.));
#7814=DIRECTION('center_axis',(0.,0.,-1.));
#7815=DIRECTION('ref_axis',(-1.,0.,0.));
#7816=DIRECTION('center_axis',(0.,0.,-1.));
#7817=DIRECTION('ref_axis',(1.,0.,0.));
#7818=DIRECTION('',(0.,0.,-1.));
#7819=DIRECTION('center_axis',(0.,0.,1.));
#7820=DIRECTION('ref_axis',(1.,0.,0.));
#7821=DIRECTION('center_axis',(0.,0.,-1.));
#7822=DIRECTION('ref_axis',(-1.,0.,0.));
#7823=DIRECTION('center_axis',(0.,0.,1.));
#7824=DIRECTION('ref_axis',(1.,0.,0.));
#7825=DIRECTION('center_axis',(0.,0.,1.));
#7826=DIRECTION('ref_axis',(1.,0.,0.));
#7827=DIRECTION('',(0.,0.,-1.));
#7828=DIRECTION('center_axis',(0.,0.,1.));
#7829=DIRECTION('ref_axis',(1.,0.,0.));
#7830=DIRECTION('',(0.,0.,-1.));
#7831=DIRECTION('center_axis',(0.,0.,1.));
#7832=DIRECTION('ref_axis',(1.,0.,0.));
#7833=DIRECTION('center_axis',(0.,0.,1.));
#7834=DIRECTION('ref_axis',(1.,0.,0.));
#7835=DIRECTION('center_axis',(0.,0.,1.));
#7836=DIRECTION('ref_axis',(1.,0.,0.));
#7837=DIRECTION('',(-1.,0.,0.));
#7838=DIRECTION('',(1.,-1.39897054514259E-17,0.));
#7839=DIRECTION('center_axis',(0.,0.,1.));
#7840=DIRECTION('ref_axis',(1.,0.,0.));
#7841=DIRECTION('',(-1.,0.,0.));
#7842=DIRECTION('',(-1.,0.,0.));
#7843=DIRECTION('center_axis',(0.,0.,-1.));
#7844=DIRECTION('ref_axis',(1.,0.,0.));
#7845=DIRECTION('',(1.,3.16619526353726E-17,0.));
#7846=DIRECTION('',(-1.,3.16619526353726E-17,0.));
#7847=DIRECTION('center_axis',(0.,0.,1.));
#7848=DIRECTION('ref_axis',(1.,0.,0.));
#7849=DIRECTION('',(-1.,0.,0.));
#7850=DIRECTION('center_axis',(0.,0.,1.));
#7851=DIRECTION('ref_axis',(1.,0.,0.));
#7852=DIRECTION('',(1.,-1.39897054514259E-17,0.));
#7853=DIRECTION('',(-1.,3.16619526353726E-17,0.));
#7854=DIRECTION('center_axis',(0.,0.,-1.));
#7855=DIRECTION('ref_axis',(1.,0.,0.));
#7856=DIRECTION('',(1.,3.16619526353726E-17,0.));
#7857=DIRECTION('center_axis',(1.39897054514259E-17,1.,0.));
#7858=DIRECTION('ref_axis',(-1.,1.39897054514259E-17,0.));
#7859=DIRECTION('',(0.,0.,-1.));
#7860=DIRECTION('center_axis',(0.,0.,-1.));
#7861=DIRECTION('ref_axis',(1.,1.22464679914735E-16,0.));
#7862=DIRECTION('',(0.,0.,-1.));
#7863=DIRECTION('center_axis',(0.,-1.,0.));
#7864=DIRECTION('ref_axis',(0.,0.,-1.));
#7865=DIRECTION('center_axis',(0.,0.,1.));
#7866=DIRECTION('ref_axis',(-1.,1.22464679914735E-16,0.));
#7867=DIRECTION('',(0.,0.,1.));
#7868=DIRECTION('center_axis',(0.,0.,-1.));
#7869=DIRECTION('ref_axis',(1.,0.,0.));
#7870=DIRECTION('',(0.,0.,1.));
#7871=DIRECTION('center_axis',(3.16619526353726E-17,-1.,0.));
#7872=DIRECTION('ref_axis',(1.,3.16619526353726E-17,0.));
#7873=DIRECTION('',(1.,3.16619526353726E-17,0.));
#7874=DIRECTION('center_axis',(3.16619526353726E-17,1.,0.));
#7875=DIRECTION('ref_axis',(-1.,3.16619526353726E-17,0.));
#7876=DIRECTION('',(-1.,3.16619526353726E-17,0.));
#7877=DIRECTION('center_axis',(0.,0.,1.));
#7878=DIRECTION('ref_axis',(1.,0.,0.));
#7879=DIRECTION('center_axis',(-3.16619526353726E-17,-1.,0.));
#7880=DIRECTION('ref_axis',(1.,-3.16619526353726E-17,0.));
#7881=DIRECTION('',(-1.,3.16619526353726E-17,0.));
#7882=DIRECTION('',(0.,0.,-1.));
#7883=DIRECTION('center_axis',(0.,0.,-1.));
#7884=DIRECTION('ref_axis',(1.,1.22464679914735E-16,0.));
#7885=DIRECTION('center_axis',(0.,0.,-1.));
#7886=DIRECTION('ref_axis',(1.,0.,0.));
#7887=DIRECTION('',(0.,0.,-1.));
#7888=DIRECTION('center_axis',(-3.16619526353726E-17,1.,0.));
#7889=DIRECTION('ref_axis',(-1.,-3.16619526353726E-17,0.));
#7890=DIRECTION('',(1.,3.16619526353726E-17,0.));
#7891=DIRECTION('center_axis',(0.,0.,-1.));
#7892=DIRECTION('ref_axis',(1.,0.,0.));
#7893=DIRECTION('center_axis',(0.,0.,1.));
#7894=DIRECTION('ref_axis',(1.,0.,0.));
#7895=DIRECTION('',(-1.,0.,0.));
#7896=DIRECTION('',(-1.,0.,0.));
#7897=DIRECTION('',(0.,-1.,0.));
#7898=DIRECTION('center_axis',(0.,-1.,0.));
#7899=DIRECTION('ref_axis',(0.,0.,-1.));
#7900=DIRECTION('',(0.,0.,-1.));
#7901=DIRECTION('',(-1.,0.,0.));
#7902=DIRECTION('',(0.,0.,-1.));
#7903=DIRECTION('center_axis',(0.,0.,-1.));
#7904=DIRECTION('ref_axis',(1.,1.22464679914735E-16,0.));
#7905=DIRECTION('',(0.,0.,-1.));
#7906=DIRECTION('center_axis',(0.,0.,1.));
#7907=DIRECTION('ref_axis',(1.,0.,0.));
#7908=DIRECTION('center_axis',(0.,-1.,0.));
#7909=DIRECTION('ref_axis',(0.,0.,-1.));
#7910=DIRECTION('',(0.,0.,-1.));
#7911=DIRECTION('',(-1.,0.,0.));
#7912=DIRECTION('center_axis',(1.,0.,0.));
#7913=DIRECTION('ref_axis',(0.,0.,-1.));
#7914=DIRECTION('',(0.,-1.,0.));
#7915=DIRECTION('center_axis',(0.,0.,1.));
#7916=DIRECTION('ref_axis',(1.,0.,0.));
#7917=DIRECTION('center_axis',(0.,0.,1.));
#7918=DIRECTION('ref_axis',(1.,0.,0.));
#7919=DIRECTION('axis',(0.,0.,1.));
#7920=DIRECTION('refdir',(1.,0.,0.));
#7921=DIRECTION('center_axis',(0.,0.,-1.));
#7922=DIRECTION('ref_axis',(-1.,0.,0.));
#7923=DIRECTION('center_axis',(0.,0.,1.));
#7924=DIRECTION('ref_axis',(1.,0.,0.));
#7925=DIRECTION('',(0.,0.,-1.));
#7926=DIRECTION('center_axis',(0.,0.,1.));
#7927=DIRECTION('ref_axis',(1.,0.,0.));
#7928=DIRECTION('center_axis',(0.,0.,-1.));
#7929=DIRECTION('ref_axis',(-1.,0.,0.));
#7930=DIRECTION('center_axis',(0.,0.,1.));
#7931=DIRECTION('ref_axis',(1.,0.,0.));
#7932=DIRECTION('',(0.,0.,-1.));
#7933=DIRECTION('center_axis',(0.,0.,1.));
#7934=DIRECTION('ref_axis',(1.,0.,0.));
#7935=DIRECTION('',(0.,0.,-1.));
#7936=DIRECTION('center_axis',(0.,0.,-1.));
#7937=DIRECTION('ref_axis',(-1.,0.,0.));
#7938=DIRECTION('center_axis',(0.,0.,1.));
#7939=DIRECTION('ref_axis',(1.,0.,0.));
#7940=DIRECTION('',(0.,0.,1.));
#7941=DIRECTION('center_axis',(0.,0.,1.));
#7942=DIRECTION('ref_axis',(1.,0.,0.));
#7943=DIRECTION('center_axis',(0.,0.,-1.));
#7944=DIRECTION('ref_axis',(-1.,0.,0.));
#7945=DIRECTION('center_axis',(0.,0.,-1.));
#7946=DIRECTION('ref_axis',(1.,0.,0.));
#7947=DIRECTION('',(0.,0.,-1.));
#7948=DIRECTION('center_axis',(0.,0.,-1.));
#7949=DIRECTION('ref_axis',(1.,0.,0.));
#7950=DIRECTION('',(0.,0.,-1.));
#7951=DIRECTION('center_axis',(0.,0.,1.));
#7952=DIRECTION('ref_axis',(1.,0.,0.));
#7953=DIRECTION('center_axis',(0.,0.,-1.));
#7954=DIRECTION('ref_axis',(1.,0.,0.));
#7955=DIRECTION('',(0.,0.,1.));
#7956=DIRECTION('center_axis',(0.,0.,-1.));
#7957=DIRECTION('ref_axis',(1.,0.,0.));
#7958=DIRECTION('',(0.,0.,1.));
#7959=DIRECTION('center_axis',(0.,0.,-1.));
#7960=DIRECTION('ref_axis',(-1.,0.,0.));
#7961=DIRECTION('center_axis',(0.,0.,-1.));
#7962=DIRECTION('ref_axis',(1.,0.,0.));
#7963=DIRECTION('',(0.,0.,-1.));
#7964=DIRECTION('center_axis',(0.,0.,1.));
#7965=DIRECTION('ref_axis',(1.,0.,0.));
#7966=DIRECTION('center_axis',(0.,0.,-1.));
#7967=DIRECTION('ref_axis',(-1.,0.,0.));
#7968=DIRECTION('center_axis',(0.,0.,-1.));
#7969=DIRECTION('ref_axis',(1.,0.,0.));
#7970=DIRECTION('',(0.,0.,-1.));
#7971=DIRECTION('center_axis',(0.,0.,1.));
#7972=DIRECTION('ref_axis',(1.,0.,0.));
#7973=DIRECTION('center_axis',(0.,0.,1.));
#7974=DIRECTION('ref_axis',(1.,0.,0.));
#7975=DIRECTION('',(1.,0.,0.));
#7976=DIRECTION('',(0.,-1.,0.));
#7977=DIRECTION('',(-1.,-1.38777878078145E-16,0.));
#7978=DIRECTION('center_axis',(0.,0.,1.));
#7979=DIRECTION('ref_axis',(1.,0.,0.));
#7980=DIRECTION('center_axis',(0.,0.,1.));
#7981=DIRECTION('ref_axis',(1.,0.,0.));
#7982=DIRECTION('',(-1.,0.,0.));
#7983=DIRECTION('',(0.,-1.,0.));
#7984=DIRECTION('',(1.,-1.39897054514259E-17,0.));
#7985=DIRECTION('center_axis',(0.,0.,1.));
#7986=DIRECTION('ref_axis',(1.,0.,0.));
#7987=DIRECTION('',(-1.,0.,0.));
#7988=DIRECTION('',(0.,-1.,0.));
#7989=DIRECTION('',(-1.,0.,0.));
#7990=DIRECTION('center_axis',(0.,0.,-1.));
#7991=DIRECTION('ref_axis',(1.,0.,0.));
#7992=DIRECTION('',(1.,3.16619526353726E-17,0.));
#7993=DIRECTION('',(-1.,3.16619526353726E-17,0.));
#7994=DIRECTION('center_axis',(0.,0.,1.));
#7995=DIRECTION('ref_axis',(1.,0.,0.));
#7996=DIRECTION('',(1.,-1.39897054514259E-17,0.));
#7997=DIRECTION('',(-1.,0.,0.));
#7998=DIRECTION('center_axis',(0.,0.,1.));
#7999=DIRECTION('ref_axis',(1.,0.,0.));
#8000=DIRECTION('',(-1.,3.16619526353726E-17,0.));
#8001=DIRECTION('center_axis',(0.,0.,-1.));
#8002=DIRECTION('ref_axis',(1.,0.,0.));
#8003=DIRECTION('',(1.,3.16619526353726E-17,0.));
#8004=DIRECTION('center_axis',(1.39897054514259E-17,1.,0.));
#8005=DIRECTION('ref_axis',(-1.,1.39897054514259E-17,0.));
#8006=DIRECTION('',(0.,0.,-1.));
#8007=DIRECTION('',(0.,0.,-1.));
#8008=DIRECTION('center_axis',(0.,0.,-1.));
#8009=DIRECTION('ref_axis',(1.,1.22464679914735E-16,0.));
#8010=DIRECTION('',(0.,0.,-1.));
#8011=DIRECTION('center_axis',(0.,-1.,0.));
#8012=DIRECTION('ref_axis',(0.,0.,-1.));
#8013=DIRECTION('',(0.,0.,-1.));
#8014=DIRECTION('center_axis',(0.,0.,1.));
#8015=DIRECTION('ref_axis',(-1.,1.22464679914735E-16,0.));
#8016=DIRECTION('',(0.,0.,1.));
#8017=DIRECTION('center_axis',(0.,0.,-1.));
#8018=DIRECTION('ref_axis',(1.,0.,0.));
#8019=DIRECTION('',(0.,0.,1.));
#8020=DIRECTION('center_axis',(3.16619526353726E-17,-1.,0.));
#8021=DIRECTION('ref_axis',(1.,3.16619526353726E-17,0.));
#8022=DIRECTION('',(1.,3.16619526353726E-17,0.));
#8023=DIRECTION('center_axis',(3.16619526353726E-17,1.,0.));
#8024=DIRECTION('ref_axis',(-1.,3.16619526353726E-17,0.));
#8025=DIRECTION('',(-1.,3.16619526353726E-17,0.));
#8026=DIRECTION('center_axis',(0.,0.,1.));
#8027=DIRECTION('ref_axis',(1.,0.,0.));
#8028=DIRECTION('center_axis',(-3.16619526353726E-17,-1.,0.));
#8029=DIRECTION('ref_axis',(1.,-3.16619526353726E-17,0.));
#8030=DIRECTION('',(-1.,3.16619526353726E-17,0.));
#8031=DIRECTION('',(0.,0.,-1.));
#8032=DIRECTION('center_axis',(0.,0.,-1.));
#8033=DIRECTION('ref_axis',(1.,1.22464679914735E-16,0.));
#8034=DIRECTION('center_axis',(0.,0.,-1.));
#8035=DIRECTION('ref_axis',(1.,0.,0.));
#8036=DIRECTION('',(0.,0.,-1.));
#8037=DIRECTION('center_axis',(-3.16619526353726E-17,1.,0.));
#8038=DIRECTION('ref_axis',(-1.,-3.16619526353726E-17,0.));
#8039=DIRECTION('',(1.,3.16619526353726E-17,0.));
#8040=DIRECTION('center_axis',(0.,0.,-1.));
#8041=DIRECTION('ref_axis',(1.,0.,0.));
#8042=DIRECTION('center_axis',(0.,-1.,0.));
#8043=DIRECTION('ref_axis',(0.,0.,-1.));
#8044=DIRECTION('',(0.,0.,-1.));
#8045=DIRECTION('',(-1.,0.,0.));
#8046=DIRECTION('',(0.,0.,-1.));
#8047=DIRECTION('center_axis',(0.,0.,-1.));
#8048=DIRECTION('ref_axis',(1.,1.22464679914735E-16,0.));
#8049=DIRECTION('',(0.,0.,-1.));
#8050=DIRECTION('center_axis',(0.,0.,1.));
#8051=DIRECTION('ref_axis',(1.,0.,0.));
#8052=DIRECTION('center_axis',(0.,-1.,0.));
#8053=DIRECTION('ref_axis',(0.,0.,-1.));
#8054=DIRECTION('',(0.,0.,-1.));
#8055=DIRECTION('',(-1.,0.,0.));
#8056=DIRECTION('center_axis',(1.,0.,0.));
#8057=DIRECTION('ref_axis',(0.,0.,-1.));
#8058=DIRECTION('',(0.,-1.,0.));
#8059=DIRECTION('center_axis',(0.,0.,1.));
#8060=DIRECTION('ref_axis',(1.,0.,0.));
#8061=DIRECTION('center_axis',(0.,0.,1.));
#8062=DIRECTION('ref_axis',(1.,0.,0.));
#8063=DIRECTION('axis',(0.,0.,1.));
#8064=DIRECTION('refdir',(1.,0.,0.));
#8065=DIRECTION('center_axis',(0.,0.,1.));
#8066=DIRECTION('ref_axis',(-1.83697019872103E-16,-1.,0.));
#8067=DIRECTION('center_axis',(0.,0.,1.));
#8068=DIRECTION('ref_axis',(1.,0.,0.));
#8069=DIRECTION('',(0.,0.,1.));
#8070=DIRECTION('center_axis',(0.,0.,1.));
#8071=DIRECTION('ref_axis',(1.,0.,0.));
#8072=DIRECTION('',(0.,0.,1.));
#8073=DIRECTION('center_axis',(0.,0.,-1.));
#8074=DIRECTION('ref_axis',(-1.,0.,0.));
#8075=DIRECTION('center_axis',(0.,0.,-1.));
#8076=DIRECTION('ref_axis',(-1.,0.,0.));
#8077=DIRECTION('',(0.,0.,1.));
#8078=DIRECTION('center_axis',(0.,0.,1.));
#8079=DIRECTION('ref_axis',(1.,0.,0.));
#8080=DIRECTION('',(0.,0.,-1.));
#8081=DIRECTION('center_axis',(0.,0.,1.));
#8082=DIRECTION('ref_axis',(1.,0.,0.));
#8083=DIRECTION('center_axis',(0.,0.,-1.));
#8084=DIRECTION('ref_axis',(-1.,0.,0.));
#8085=DIRECTION('',(0.,0.,-1.));
#8086=DIRECTION('center_axis',(0.,0.,-1.));
#8087=DIRECTION('ref_axis',(-1.,0.,0.));
#8088=DIRECTION('center_axis',(0.,0.,-1.));
#8089=DIRECTION('ref_axis',(-1.,0.,0.));
#8090=DIRECTION('center_axis',(0.,0.,-1.));
#8091=DIRECTION('ref_axis',(-1.,0.,0.));
#8092=DIRECTION('',(0.,0.,1.));
#8093=DIRECTION('center_axis',(0.,0.,1.));
#8094=DIRECTION('ref_axis',(1.,0.,0.));
#8095=DIRECTION('',(0.,0.,-1.));
#8096=DIRECTION('center_axis',(0.,0.,1.));
#8097=DIRECTION('ref_axis',(1.,0.,0.));
#8098=DIRECTION('center_axis',(0.,0.,-1.));
#8099=DIRECTION('ref_axis',(-1.,0.,0.));
#8100=DIRECTION('',(0.,0.,-1.));
#8101=DIRECTION('center_axis',(0.,0.,-1.));
#8102=DIRECTION('ref_axis',(-1.,0.,0.));
#8103=DIRECTION('center_axis',(0.,0.,-1.));
#8104=DIRECTION('ref_axis',(-1.,0.,0.));
#8105=DIRECTION('center_axis',(0.,0.,-1.));
#8106=DIRECTION('ref_axis',(-1.,0.,0.));
#8107=DIRECTION('',(0.,0.,1.));
#8108=DIRECTION('center_axis',(0.,0.,1.));
#8109=DIRECTION('ref_axis',(1.,0.,0.));
#8110=DIRECTION('',(0.,0.,-1.));
#8111=DIRECTION('center_axis',(0.,0.,1.));
#8112=DIRECTION('ref_axis',(1.,0.,0.));
#8113=DIRECTION('center_axis',(1.34209460732156E-15,-2.06113990643666E-16,
-1.));
#8114=DIRECTION('ref_axis',(-1.,2.14280619850583E-33,-1.34209460732156E-15));
#8115=DIRECTION('center_axis',(0.,0.,-1.));
#8116=DIRECTION('ref_axis',(-1.,0.,0.));
#8117=DIRECTION('',(0.,0.,1.));
#8118=DIRECTION('center_axis',(0.,0.,-1.));
#8119=DIRECTION('ref_axis',(-1.,0.,0.));
#8120=DIRECTION('center_axis',(0.,0.,-1.));
#8121=DIRECTION('ref_axis',(-1.,0.,0.));
#8122=DIRECTION('',(0.,0.,1.));
#8123=DIRECTION('center_axis',(0.,0.,1.));
#8124=DIRECTION('ref_axis',(1.,0.,0.));
#8125=DIRECTION('',(0.,0.,-1.));
#8126=DIRECTION('center_axis',(0.,0.,1.));
#8127=DIRECTION('ref_axis',(1.,0.,0.));
#8128=DIRECTION('center_axis',(0.,0.,-1.));
#8129=DIRECTION('ref_axis',(-1.,0.,0.));
#8130=DIRECTION('center_axis',(-1.3556201284053E-15,-7.74272536198527E-17,
-1.));
#8131=DIRECTION('ref_axis',(-1.,2.42293261278703E-34,1.3556201284053E-15));
#8132=DIRECTION('',(0.,0.,1.));
#8133=DIRECTION('center_axis',(0.,0.,-1.));
#8134=DIRECTION('ref_axis',(-1.,0.,0.));
#8135=DIRECTION('center_axis',(0.,0.,-1.));
#8136=DIRECTION('ref_axis',(-1.,0.,0.));
#8137=DIRECTION('',(0.,0.,1.));
#8138=DIRECTION('center_axis',(0.,0.,1.));
#8139=DIRECTION('ref_axis',(1.,0.,0.));
#8140=DIRECTION('',(0.,0.,-1.));
#8141=DIRECTION('center_axis',(0.,0.,-1.));
#8142=DIRECTION('ref_axis',(-1.,0.,0.));
#8143=DIRECTION('center_axis',(0.,0.,-1.));
#8144=DIRECTION('ref_axis',(-1.,0.,0.));
#8145=DIRECTION('',(0.,0.,1.));
#8146=DIRECTION('center_axis',(0.,0.,1.));
#8147=DIRECTION('ref_axis',(1.,0.,0.));
#8148=DIRECTION('',(0.,0.,-1.));
#8149=DIRECTION('center_axis',(0.,0.,-1.));
#8150=DIRECTION('ref_axis',(-1.,0.,0.));
#8151=DIRECTION('center_axis',(-2.13696732994728E-15,-4.30864304074819E-16,
-1.));
#8152=DIRECTION('ref_axis',(-1.,-1.17354868605786E-31,2.13696732994728E-15));
#8153=DIRECTION('',(0.,0.,1.));
#8154=DIRECTION('center_axis',(-2.13696732994728E-15,-4.30864304074819E-16,
1.));
#8155=DIRECTION('ref_axis',(1.,1.17354868605786E-31,2.13696732994728E-15));
#8156=DIRECTION('',(0.,0.,-1.));
#8157=DIRECTION('center_axis',(0.,0.,-1.));
#8158=DIRECTION('ref_axis',(-1.,0.,0.));
#8159=DIRECTION('center_axis',(0.,0.,-1.));
#8160=DIRECTION('ref_axis',(-1.,0.,0.));
#8161=DIRECTION('',(0.,0.,1.));
#8162=DIRECTION('center_axis',(0.,0.,1.));
#8163=DIRECTION('ref_axis',(1.,0.,0.));
#8164=DIRECTION('',(0.,0.,-1.));
#8165=DIRECTION('center_axis',(0.,0.,-1.));
#8166=DIRECTION('ref_axis',(-1.,0.,0.));
#8167=DIRECTION('center_axis',(1.77696849674338E-15,1.26279704599331E-15,
-1.));
#8168=DIRECTION('ref_axis',(-1.,2.15613826771123E-31,-1.77696849674338E-15));
#8169=DIRECTION('',(0.,0.,1.));
#8170=DIRECTION('center_axis',(1.77696849674338E-15,1.26279704599331E-15,
1.));
#8171=DIRECTION('ref_axis',(1.,-2.15613826771123E-31,-1.77696849674338E-15));
#8172=DIRECTION('',(0.,0.,-1.));
#8173=DIRECTION('center_axis',(0.,0.,-1.));
#8174=DIRECTION('ref_axis',(-1.,0.,0.));
#8175=DIRECTION('center_axis',(0.,0.,-1.));
#8176=DIRECTION('ref_axis',(-1.,0.,0.));
#8177=DIRECTION('',(0.,0.,1.));
#8178=DIRECTION('center_axis',(0.,0.,1.));
#8179=DIRECTION('ref_axis',(1.,0.,0.));
#8180=DIRECTION('',(0.,0.,-1.));
#8181=DIRECTION('center_axis',(0.,0.,-1.));
#8182=DIRECTION('ref_axis',(-1.,0.,0.));
#8183=DIRECTION('center_axis',(0.,0.,-1.));
#8184=DIRECTION('ref_axis',(-1.,0.,0.));
#8185=DIRECTION('',(0.,0.,1.));
#8186=DIRECTION('center_axis',(0.,0.,1.));
#8187=DIRECTION('ref_axis',(1.,0.,0.));
#8188=DIRECTION('',(0.,0.,-1.));
#8189=DIRECTION('center_axis',(0.,0.,-1.));
#8190=DIRECTION('ref_axis',(-1.,0.,0.));
#8191=DIRECTION('center_axis',(0.,0.,-1.));
#8192=DIRECTION('ref_axis',(-1.,0.,0.));
#8193=DIRECTION('',(0.,0.,1.));
#8194=DIRECTION('center_axis',(0.,0.,1.));
#8195=DIRECTION('ref_axis',(1.,0.,0.));
#8196=DIRECTION('',(0.,0.,-1.));
#8197=DIRECTION('center_axis',(0.,0.,-1.));
#8198=DIRECTION('ref_axis',(-1.,0.,0.));
#8199=DIRECTION('center_axis',(-2.13696732994721E-15,4.30864304074825E-16,
-1.));
#8200=DIRECTION('ref_axis',(-1.,1.17354868605837E-31,2.13696732994721E-15));
#8201=DIRECTION('',(0.,0.,1.));
#8202=DIRECTION('center_axis',(-2.13696732994721E-15,4.30864304074825E-16,
1.));
#8203=DIRECTION('ref_axis',(1.,-1.17354868605837E-31,2.13696732994721E-15));
#8204=DIRECTION('',(0.,0.,-1.));
#8205=DIRECTION('center_axis',(0.,0.,-1.));
#8206=DIRECTION('ref_axis',(-1.,0.,0.));
#8207=DIRECTION('center_axis',(0.,0.,-1.));
#8208=DIRECTION('ref_axis',(-1.,0.,0.));
#8209=DIRECTION('',(0.,0.,1.));
#8210=DIRECTION('center_axis',(0.,0.,1.));
#8211=DIRECTION('ref_axis',(1.,0.,0.));
#8212=DIRECTION('',(0.,0.,-1.));
#8213=DIRECTION('center_axis',(0.,0.,-1.));
#8214=DIRECTION('ref_axis',(-1.,0.,0.));
#8215=DIRECTION('center_axis',(-3.9743489494276E-14,0.,1.));
#8216=DIRECTION('ref_axis',(1.,0.,3.9743489494276E-14));
#8217=DIRECTION('',(0.,0.,-1.));
#8218=DIRECTION('center_axis',(3.9743489494276E-14,0.,1.));
#8219=DIRECTION('ref_axis',(1.,0.,-3.9743489494276E-14));
#8220=DIRECTION('',(0.,0.,1.));
#8221=DIRECTION('center_axis',(0.,0.,-1.));
#8222=DIRECTION('ref_axis',(-1.,0.,0.));
#8223=DIRECTION('center_axis',(-2.65935852241228E-14,-2.95351685640873E-14,
1.));
#8224=DIRECTION('ref_axis',(1.52054869890062E-31,-1.,-2.95351685640873E-14));
#8225=DIRECTION('',(0.,0.,-1.));
#8226=DIRECTION('center_axis',(2.65935852241255E-14,2.95351685640904E-14,
1.));
#8227=DIRECTION('ref_axis',(1.52054870042792E-31,-1.,2.95351685640904E-14));
#8228=DIRECTION('',(0.,0.,1.));
#8229=DIRECTION('center_axis',(0.,0.,-1.));
#8230=DIRECTION('ref_axis',(-1.,0.,0.));
#8231=DIRECTION('center_axis',(3.21531584166429E-14,2.33606369993845E-14,
1.));
#8232=DIRECTION('ref_axis',(1.,-8.29846859020713E-32,-3.21531584166429E-14));
#8233=DIRECTION('',(0.,0.,1.));
#8234=DIRECTION('center_axis',(-3.21531584166387E-14,-2.33606369993815E-14,
1.));
#8235=DIRECTION('ref_axis',(1.,-8.29846856946285E-32,3.21531584166387E-14));
#8236=DIRECTION('',(0.,0.,-1.));
#8237=DIRECTION('center_axis',(0.,0.,-1.));
#8238=DIRECTION('ref_axis',(-1.,0.,0.));
#8239=DIRECTION('center_axis',(-1.98717447471412E-14,-3.44188715370884E-14,
1.));
#8240=DIRECTION('ref_axis',(-9.03655535160673E-32,-1.,-3.44188715370884E-14));
#8241=DIRECTION('',(0.,0.,-1.));
#8242=DIRECTION('center_axis',(1.98717447471412E-14,3.44188715370884E-14,
1.));
#8243=DIRECTION('ref_axis',(-9.03655535160673E-32,-1.,3.44188715370884E-14));
#8244=DIRECTION('',(0.,0.,1.));
#8245=DIRECTION('center_axis',(0.,0.,-1.));
#8246=DIRECTION('ref_axis',(-1.,0.,0.));
#8247=DIRECTION('center_axis',(-1.22814136694924E-14,-3.77983046638355E-14,
1.));
#8248=DIRECTION('ref_axis',(2.22571381162951E-32,-1.,-3.77983046638355E-14));
#8249=DIRECTION('',(0.,0.,-1.));
#8250=DIRECTION('center_axis',(1.22814136694963E-14,3.7798304663847E-14,
1.));
#8251=DIRECTION('ref_axis',(2.22571383838198E-32,-1.,3.7798304663847E-14));
#8252=DIRECTION('',(0.,0.,1.));
#8253=DIRECTION('center_axis',(0.,0.,-1.));
#8254=DIRECTION('ref_axis',(-1.,0.,0.));
#8255=DIRECTION('center_axis',(3.63074842983588E-14,1.61651335010186E-14,
1.));
#8256=DIRECTION('ref_axis',(1.,-2.86104045702539E-32,-3.63074842983588E-14));
#8257=DIRECTION('',(0.,0.,1.));
#8258=DIRECTION('center_axis',(-3.63074842983588E-14,-1.61651335010186E-14,
1.));
#8259=DIRECTION('ref_axis',(1.,-2.86104045702539E-32,3.63074842983588E-14));
#8260=DIRECTION('',(0.,0.,-1.));
#8261=DIRECTION('center_axis',(0.,0.,-1.));
#8262=DIRECTION('ref_axis',(-1.,0.,0.));
#8263=DIRECTION('center_axis',(3.88749988936205E-14,8.263136099754E-15,
1.));
#8264=DIRECTION('ref_axis',(1.,4.7064185543995E-32,-3.88749988936205E-14));
#8265=DIRECTION('',(0.,0.,1.));
#8266=DIRECTION('center_axis',(-3.88749988936141E-14,-8.26313609975264E-15,
1.));
#8267=DIRECTION('ref_axis',(1.,4.70641856382513E-32,3.88749988936141E-14));
#8268=DIRECTION('',(0.,0.,-1.));
#8269=DIRECTION('center_axis',(0.,0.,-1.));
#8270=DIRECTION('ref_axis',(-1.,0.,0.));
#8271=DIRECTION('center_axis',(3.88749988936198E-14,-8.26313609975388E-15,
1.));
#8272=DIRECTION('ref_axis',(1.,-4.70641855550782E-32,-3.88749988936198E-14));
#8273=DIRECTION('',(0.,0.,1.));
#8274=DIRECTION('center_axis',(-3.88749988936198E-14,8.2631360997538E-15,
1.));
#8275=DIRECTION('ref_axis',(1.,-4.70641855495463E-32,3.88749988936198E-14));
#8276=DIRECTION('',(0.,0.,-1.));
#8277=DIRECTION('center_axis',(0.,0.,-1.));
#8278=DIRECTION('ref_axis',(-1.,0.,0.));
#8279=DIRECTION('center_axis',(-1.98717447471421E-14,3.44188715370906E-14,
1.));
#8280=DIRECTION('ref_axis',(9.03655534251286E-32,-1.,3.44188715370906E-14));
#8281=DIRECTION('',(0.,0.,-1.));
#8282=DIRECTION('center_axis',(1.98717447471421E-14,-3.44188715370906E-14,
1.));
#8283=DIRECTION('ref_axis',(9.03655534251286E-32,-1.,-3.44188715370906E-14));
#8284=DIRECTION('',(0.,0.,1.));
#8285=DIRECTION('center_axis',(0.,0.,-1.));
#8286=DIRECTION('ref_axis',(-1.,0.,0.));
#8287=DIRECTION('center_axis',(-2.65935852241256E-14,2.95351685640909E-14,
1.));
#8288=DIRECTION('ref_axis',(-1.52054870064765E-31,-1.,2.95351685640909E-14));
#8289=DIRECTION('',(0.,0.,-1.));
#8290=DIRECTION('center_axis',(2.65935852241255E-14,-2.95351685640905E-14,
1.));
#8291=DIRECTION('ref_axis',(-1.52054870032748E-31,-1.,-2.95351685640905E-14));
#8292=DIRECTION('',(0.,0.,1.));
#8293=DIRECTION('center_axis',(0.,0.,-1.));
#8294=DIRECTION('ref_axis',(-1.,0.,0.));
#8295=DIRECTION('center_axis',(3.6307484298364E-14,-1.61651335010211E-14,
1.));
#8296=DIRECTION('ref_axis',(1.,2.86104047421028E-32,-3.6307484298364E-14));
#8297=DIRECTION('',(0.,0.,1.));
#8298=DIRECTION('center_axis',(-3.6307484298364E-14,1.61651335010213E-14,
1.));
#8299=DIRECTION('ref_axis',(1.,2.86104047531475E-32,3.6307484298364E-14));
#8300=DIRECTION('',(0.,0.,-1.));
#8301=DIRECTION('center_axis',(0.,0.,-1.));
#8302=DIRECTION('ref_axis',(-1.,0.,0.));
#8303=DIRECTION('center_axis',(3.21531584166325E-14,-2.33606369993773E-14,
1.));
#8304=DIRECTION('ref_axis',(1.,8.29846854034834E-32,-3.21531584166325E-14));
#8305=DIRECTION('',(0.,0.,1.));
#8306=DIRECTION('center_axis',(-3.21531584166325E-14,2.33606369993773E-14,
1.));
#8307=DIRECTION('ref_axis',(1.,8.29846854034834E-32,3.21531584166325E-14));
#8308=DIRECTION('',(0.,0.,-1.));
#8309=DIRECTION('center_axis',(0.,0.,-1.));
#8310=DIRECTION('ref_axis',(-1.,0.,0.));
#8311=DIRECTION('center_axis',(1.22814136694964E-14,-3.77983046638479E-14,
1.));
#8312=DIRECTION('ref_axis',(-2.22571383991556E-32,-1.,-3.77983046638479E-14));
#8313=DIRECTION('',(0.,0.,1.));
#8314=DIRECTION('center_axis',(-1.2281413669496E-14,3.7798304663847E-14,
1.));
#8315=DIRECTION('ref_axis',(-2.22571383826539E-32,-1.,3.7798304663847E-14));
#8316=DIRECTION('',(0.,0.,-1.));
#8317=DIRECTION('center_axis',(0.,0.,-1.));
#8318=DIRECTION('ref_axis',(-1.,0.,0.));
#8319=DIRECTION('center_axis',(4.15432588173347E-15,-3.95257705004224E-14,
1.));
#8320=DIRECTION('ref_axis',(1.01104027071865E-32,-1.,-3.95257705004224E-14));
#8321=DIRECTION('',(0.,0.,1.));
#8322=DIRECTION('center_axis',(-4.15432588173344E-15,3.95257705004224E-14,
1.));
#8323=DIRECTION('ref_axis',(1.01104027037785E-32,-1.,3.95257705004224E-14));
#8324=DIRECTION('',(0.,0.,-1.));
#8325=DIRECTION('center_axis',(0.,0.,-1.));
#8326=DIRECTION('ref_axis',(-1.,0.,0.));
#8327=DIRECTION('center_axis',(-4.15432588173031E-15,-3.95257705003908E-14,
1.));
#8328=DIRECTION('ref_axis',(-1.01104028749611E-32,-1.,-3.95257705003908E-14));
#8329=DIRECTION('',(0.,0.,1.));
#8330=DIRECTION('center_axis',(4.1543258817303E-15,3.95257705003909E-14,
1.));
#8331=DIRECTION('ref_axis',(-1.0110402872876E-32,-1.,3.95257705003909E-14));
#8332=DIRECTION('center_axis',(0.,0.,-1.));
#8333=DIRECTION('ref_axis',(-1.,0.,0.));
#8334=DIRECTION('center_axis',(-1.22814136694946E-14,-3.77983046638411E-14,
1.));
#8335=DIRECTION('ref_axis',(2.22571382356633E-32,-1.,-3.77983046638411E-14));
#8336=DIRECTION('',(0.,0.,1.));
#8337=DIRECTION('center_axis',(1.22814136694949E-14,3.77983046638421E-14,
1.));
#8338=DIRECTION('ref_axis',(2.2257138263465E-32,-1.,3.77983046638421E-14));
#8339=DIRECTION('center_axis',(0.,0.,-1.));
#8340=DIRECTION('ref_axis',(-1.,0.,0.));
#8341=DIRECTION('center_axis',(1.22814136694957E-14,-3.77983046638471E-14,
1.));
#8342=DIRECTION('ref_axis',(-2.22571383862412E-32,-1.,-3.77983046638471E-14));
#8343=DIRECTION('',(0.,0.,-1.));
#8344=DIRECTION('center_axis',(-1.22814136694957E-14,3.77983046638471E-14,
1.));
#8345=DIRECTION('ref_axis',(-2.22571383862412E-32,-1.,3.77983046638471E-14));
#8346=DIRECTION('center_axis',(0.,0.,-1.));
#8347=DIRECTION('ref_axis',(-1.,0.,0.));
#8348=DIRECTION('center_axis',(1.9871744747142E-14,-3.44188715370905E-14,
1.));
#8349=DIRECTION('ref_axis',(9.03655534124833E-32,-1.,-3.44188715370905E-14));
#8350=DIRECTION('',(0.,0.,-1.));
#8351=DIRECTION('center_axis',(-1.98717447471409E-14,3.44188715370886E-14,
1.));
#8352=DIRECTION('ref_axis',(9.03655535174126E-32,-1.,3.44188715370886E-14));
#8353=DIRECTION('',(0.,0.,1.));
#8354=DIRECTION('center_axis',(0.,0.,-1.));
#8355=DIRECTION('ref_axis',(-1.,0.,0.));
#8356=DIRECTION('center_axis',(3.21531584166354E-14,-2.33606369993796E-14,
1.));
#8357=DIRECTION('ref_axis',(1.,8.29846855706183E-32,-3.21531584166354E-14));
#8358=DIRECTION('',(0.,0.,-1.));
#8359=DIRECTION('center_axis',(-3.21531584166371E-14,2.33606369993811E-14,
1.));
#8360=DIRECTION('ref_axis',(1.,8.29846856272883E-32,3.21531584166371E-14));
#8361=DIRECTION('',(0.,0.,1.));
#8362=DIRECTION('center_axis',(0.,0.,-1.));
#8363=DIRECTION('ref_axis',(-1.,0.,0.));
#8364=DIRECTION('center_axis',(-2.65935852241255E-14,2.9535168564091E-14,
1.));
#8365=DIRECTION('ref_axis',(-1.52054870065482E-31,-1.,2.9535168564091E-14));
#8366=DIRECTION('',(0.,0.,1.));
#8367=DIRECTION('center_axis',(2.65935852241255E-14,-2.9535168564091E-14,
1.));
#8368=DIRECTION('ref_axis',(-1.52054870065482E-31,-1.,-2.9535168564091E-14));
#8369=DIRECTION('',(0.,0.,-1.));
#8370=DIRECTION('center_axis',(0.,0.,-1.));
#8371=DIRECTION('ref_axis',(-1.,0.,0.));
#8372=DIRECTION('center_axis',(3.6307484298364E-14,-1.61651335010214E-14,
1.));
#8373=DIRECTION('ref_axis',(1.,2.86104047630569E-32,-3.6307484298364E-14));
#8374=DIRECTION('',(0.,0.,-1.));
#8375=DIRECTION('center_axis',(-3.6307484298364E-14,1.61651335010214E-14,
1.));
#8376=DIRECTION('ref_axis',(1.,2.86104047630569E-32,3.6307484298364E-14));
#8377=DIRECTION('',(0.,0.,1.));
#8378=DIRECTION('center_axis',(0.,0.,-1.));
#8379=DIRECTION('ref_axis',(-1.,0.,0.));
#8380=DIRECTION('center_axis',(3.8874998893626E-14,-8.26313609975566E-15,
1.));
#8381=DIRECTION('ref_axis',(1.,-4.7064185451803E-32,-3.8874998893626E-14));
#8382=DIRECTION('',(0.,0.,-1.));
#8383=DIRECTION('center_axis',(-3.8874998893626E-14,8.26313609975566E-15,
1.));
#8384=DIRECTION('ref_axis',(1.,-4.7064185451803E-32,3.8874998893626E-14));
#8385=DIRECTION('',(0.,0.,1.));
#8386=DIRECTION('center_axis',(0.,0.,-1.));
#8387=DIRECTION('ref_axis',(1.,-1.00915871466367E-14,0.));
#8388=DIRECTION('center_axis',(3.9743489494276E-14,-6.0250801316063E-28,
1.));
#8389=DIRECTION('ref_axis',(1.,2.69212629025427E-45,-3.9743489494276E-14));
#8390=DIRECTION('',(0.,0.,-1.));
#8391=DIRECTION('center_axis',(-3.9743489494276E-14,6.0250801316063E-28,
1.));
#8392=DIRECTION('ref_axis',(1.,2.69212629025427E-45,3.9743489494276E-14));
#8393=DIRECTION('',(0.,0.,1.));
#8394=DIRECTION('center_axis',(0.,0.,-1.));
#8395=DIRECTION('ref_axis',(-1.,0.,0.));
#8396=DIRECTION('center_axis',(3.88749988936263E-14,8.26313609975447E-15,
1.));
#8397=DIRECTION('ref_axis',(1.,4.70641854477592E-32,-3.88749988936263E-14));
#8398=DIRECTION('',(0.,0.,-1.));
#8399=DIRECTION('center_axis',(-3.88749988936202E-14,-8.26313609975338E-15,
1.));
#8400=DIRECTION('ref_axis',(1.,4.70641855525022E-32,3.88749988936202E-14));
#8401=DIRECTION('',(0.,0.,1.));
#8402=DIRECTION('center_axis',(0.,0.,-1.));
#8403=DIRECTION('ref_axis',(-1.,0.,0.));
#8404=DIRECTION('center_axis',(2.65935852241261E-14,2.95351685640905E-14,
1.));
#8405=DIRECTION('ref_axis',(1.52054870048981E-31,-1.,2.95351685640905E-14));
#8406=DIRECTION('',(0.,0.,-1.));
#8407=DIRECTION('center_axis',(-2.65935852241231E-14,-2.9535168564087E-14,
1.));
#8408=DIRECTION('ref_axis',(1.52054869867193E-31,-1.,-2.9535168564087E-14));
#8409=DIRECTION('',(0.,0.,1.));
#8410=DIRECTION('center_axis',(0.,0.,-1.));
#8411=DIRECTION('ref_axis',(-1.,0.,0.));
#8412=DIRECTION('center_axis',(-1.98717447471434E-14,-3.44188715370916E-14,
1.));
#8413=DIRECTION('ref_axis',(-9.03655533788522E-32,-1.,-3.44188715370916E-14));
#8414=DIRECTION('',(0.,0.,1.));
#8415=DIRECTION('center_axis',(1.98717447471426E-14,3.44188715370902E-14,
1.));
#8416=DIRECTION('ref_axis',(-9.03655534129317E-32,-1.,3.44188715370902E-14));
#8417=DIRECTION('',(0.,0.,-1.));
#8418=DIRECTION('center_axis',(0.,0.,-1.));
#8419=DIRECTION('ref_axis',(-1.,0.,0.));
#8420=DIRECTION('center_axis',(-3.21531584166418E-14,-2.33606369993834E-14,
1.));
#8421=DIRECTION('ref_axis',(1.,-8.29846858379378E-32,3.21531584166418E-14));
#8422=DIRECTION('',(0.,0.,1.));
#8423=DIRECTION('center_axis',(3.21531584166388E-14,2.33606369993814E-14,
1.));
#8424=DIRECTION('ref_axis',(1.,-8.2984685715573E-32,-3.21531584166388E-14));
#8425=DIRECTION('',(0.,0.,-1.));
#8426=DIRECTION('center_axis',(0.,0.,-1.));
#8427=DIRECTION('ref_axis',(-1.,0.,0.));
#8428=DIRECTION('center_axis',(-3.63074842983631E-14,-1.616513350102E-14,
1.));
#8429=DIRECTION('ref_axis',(1.,-2.86104047041744E-32,3.63074842983631E-14));
#8430=DIRECTION('',(0.,0.,1.));
#8431=DIRECTION('center_axis',(3.63074842983642E-14,1.61651335010208E-14,
1.));
#8432=DIRECTION('ref_axis',(1.,-2.86104047448254E-32,-3.63074842983642E-14));
#8433=DIRECTION('',(0.,0.,-1.));
#8434=DIRECTION('center_axis',(0.,0.,-1.));
#8435=DIRECTION('ref_axis',(-1.,0.,0.));
#8436=DIRECTION('center_axis',(-4.15432588173083E-15,-3.95257705003972E-14,
1.));
#8437=DIRECTION('ref_axis',(-1.01104028692887E-32,-1.,-3.95257705003972E-14));
#8438=DIRECTION('',(0.,0.,-1.));
#8439=DIRECTION('center_axis',(4.15432588173083E-15,3.95257705003972E-14,
1.));
#8440=DIRECTION('ref_axis',(-1.01104028692887E-32,-1.,3.95257705003972E-14));
#8441=DIRECTION('',(0.,0.,1.));
#8442=DIRECTION('center_axis',(0.,0.,1.));
#8443=DIRECTION('ref_axis',(1.,0.,0.));
#8444=DIRECTION('center_axis',(-1.20692810937362E-15,6.22113696155732E-16,
-1.));
#8445=DIRECTION('ref_axis',(-1.,1.73910758130641E-32,1.20692810937362E-15));
#8446=DIRECTION('center_axis',(2.17985119260763E-15,2.28516055189852E-17,
1.));
#8447=DIRECTION('ref_axis',(1.,5.24414567525364E-33,-2.17985119260763E-15));
#8448=DIRECTION('center_axis',(0.,0.,-1.));
#8449=DIRECTION('ref_axis',(-1.,0.,0.));
#8450=DIRECTION('center_axis',(0.,0.,1.));
#8451=DIRECTION('ref_axis',(1.,0.,0.));
#8452=DIRECTION('center_axis',(0.,0.,-1.));
#8453=DIRECTION('ref_axis',(-1.,0.,0.));
#8454=DIRECTION('center_axis',(0.,0.,-1.));
#8455=DIRECTION('ref_axis',(-1.,0.,0.));
#8456=DIRECTION('center_axis',(0.,0.,1.));
#8457=DIRECTION('ref_axis',(1.,0.,0.));
#8458=DIRECTION('center_axis',(0.,0.,-1.));
#8459=DIRECTION('ref_axis',(-1.,0.,0.));
#8460=DIRECTION('center_axis',(0.,0.,1.));
#8461=DIRECTION('ref_axis',(1.,0.,0.));
#8462=DIRECTION('center_axis',(2.18703987820093E-16,-1.34010054766509E-15,
-1.));
#8463=DIRECTION('ref_axis',(-2.70980336596394E-33,1.,-1.34010054766509E-15));
#8464=DIRECTION('center_axis',(0.,0.,-1.));
#8465=DIRECTION('ref_axis',(-1.,0.,0.));
#8466=DIRECTION('center_axis',(0.,0.,1.));
#8467=DIRECTION('ref_axis',(1.,0.,0.));
#8468=DIRECTION('center_axis',(0.,0.,-1.));
#8469=DIRECTION('ref_axis',(-1.,0.,0.));
#8470=DIRECTION('center_axis',(0.,0.,1.));
#8471=DIRECTION('ref_axis',(1.,0.,0.));
#8472=DIRECTION('center_axis',(-6.4697789773716E-17,-1.35628725133693E-15,
-1.));
#8473=DIRECTION('ref_axis',(-2.45620303515543E-34,1.,-1.35628725133693E-15));
#8474=DIRECTION('center_axis',(0.,0.,-1.));
#8475=DIRECTION('ref_axis',(-1.,0.,0.));
#8476=DIRECTION('center_axis',(1.77696849674338E-15,-1.26279704599333E-15,
1.));
#8477=DIRECTION('ref_axis',(1.,2.1561382677115E-31,-1.77696849674338E-15));
#8478=DIRECTION('center_axis',(0.,0.,-1.));
#8479=DIRECTION('ref_axis',(-1.,0.,0.));
#8480=DIRECTION('center_axis',(1.47558720267693E-15,1.6046544254399E-15,
1.));
#8481=DIRECTION('ref_axis',(-2.31817004142331E-33,-1.,1.6046544254399E-15));
#8482=DIRECTION('center_axis',(0.,0.,-1.));
#8483=DIRECTION('ref_axis',(-1.,0.,0.));
#8484=DIRECTION('center_axis',(0.,0.,-1.));
#8485=DIRECTION('ref_axis',(-1.,0.,0.));
#8486=DIRECTION('center_axis',(0.,0.,1.));
#8487=DIRECTION('ref_axis',(1.,0.,0.));
#8488=DIRECTION('center_axis',(0.,0.,-1.));
#8489=DIRECTION('ref_axis',(-1.,0.,0.));
#8490=DIRECTION('center_axis',(0.,0.,1.));
#8491=DIRECTION('ref_axis',(1.,0.,0.));
#8492=DIRECTION('center_axis',(-6.10756095622581E-16,-1.21271509589043E-15,
-1.));
#8493=DIRECTION('ref_axis',(1.35391388547336E-32,1.,-1.21271509589043E-15));
#8494=DIRECTION('center_axis',(-6.46977897737062E-17,1.35628725133693E-15,
-1.));
#8495=DIRECTION('ref_axis',(2.45620303514854E-34,1.,1.35628725133693E-15));
#8496=DIRECTION('center_axis',(0.,0.,1.));
#8497=DIRECTION('ref_axis',(1.,0.,0.));
#8498=DIRECTION('center_axis',(0.,0.,-1.));
#8499=DIRECTION('ref_axis',(-1.,0.,0.));
#8500=DIRECTION('center_axis',(0.,0.,1.));
#8501=DIRECTION('ref_axis',(1.,0.,0.));
#8502=DIRECTION('center_axis',(0.,0.,-1.));
#8503=DIRECTION('ref_axis',(-1.,0.,0.));
#8504=DIRECTION('center_axis',(2.18703987820102E-16,1.34010054766509E-15,
-1.));
#8505=DIRECTION('ref_axis',(2.70980336596319E-33,1.,1.34010054766509E-15));
#8506=DIRECTION('center_axis',(0.,0.,1.));
#8507=DIRECTION('ref_axis',(1.,0.,0.));
#8508=DIRECTION('center_axis',(0.,0.,-1.));
#8509=DIRECTION('ref_axis',(-1.,0.,0.));
#8510=DIRECTION('center_axis',(0.,0.,1.));
#8511=DIRECTION('ref_axis',(1.,0.,0.));
#8512=DIRECTION('center_axis',(0.,0.,-1.));
#8513=DIRECTION('ref_axis',(-1.,0.,0.));
#8514=DIRECTION('center_axis',(4.92547351688005E-16,1.2653450195444E-15,
-1.));
#8515=DIRECTION('ref_axis',(1.39597070338658E-32,1.,1.2653450195444E-15));
#8516=DIRECTION('center_axis',(2.50582917348385E-16,-2.16552109648485E-15,
1.));
#8517=DIRECTION('ref_axis',(6.10963913452889E-32,-1.,-2.16552109648485E-15));
#8518=DIRECTION('center_axis',(0.,0.,-1.));
#8519=DIRECTION('ref_axis',(-1.,0.,0.));
#8520=DIRECTION('center_axis',(0.,0.,1.));
#8521=DIRECTION('ref_axis',(1.,0.,0.));
#8522=DIRECTION('center_axis',(-1.2069281093736E-15,-6.22113696155711E-16,
-1.));
#8523=DIRECTION('ref_axis',(-1.,-1.73910758130846E-32,1.2069281093736E-15));
#8524=DIRECTION('center_axis',(0.,0.,-1.));
#8525=DIRECTION('ref_axis',(-1.,0.,0.));
#8526=DIRECTION('center_axis',(0.,0.,1.));
#8527=DIRECTION('ref_axis',(1.,0.,0.));
#8528=DIRECTION('center_axis',(0.,0.,-1.));
#8529=DIRECTION('ref_axis',(-1.,0.,0.));
#8530=DIRECTION('center_axis',(0.,0.,1.));
#8531=DIRECTION('ref_axis',(1.,0.,0.));
#8532=DIRECTION('center_axis',(0.,0.,-1.));
#8533=DIRECTION('ref_axis',(-1.,0.,0.));
#8534=DIRECTION('center_axis',(9.64626581390641E-16,9.5561313857402E-16,
-1.));
#8535=DIRECTION('ref_axis',(-1.,2.270861517335E-32,-9.64626581390641E-16));
#8536=DIRECTION('center_axis',(0.,0.,1.));
#8537=DIRECTION('ref_axis',(1.,0.,0.));
#8538=DIRECTION('center_axis',(0.,0.,-1.));
#8539=DIRECTION('ref_axis',(-1.,0.,0.));
#8540=DIRECTION('center_axis',(0.,0.,1.));
#8541=DIRECTION('ref_axis',(1.,0.,0.));
#8542=DIRECTION('center_axis',(-1.35562012840529E-15,-7.74272536198608E-17,
-1.));
#8543=DIRECTION('ref_axis',(-1.,2.42293261278864E-34,1.35562012840529E-15));
#8544=DIRECTION('center_axis',(1.1422303195999E-15,7.34173555181198E-16,
-1.));
#8545=DIRECTION('ref_axis',(-1.,1.83215133257466E-32,-1.1422303195999E-15));
#8546=DIRECTION('center_axis',(0.,0.,1.));
#8547=DIRECTION('ref_axis',(1.,0.,0.));
#8548=DIRECTION('center_axis',(0.,0.,-1.));
#8549=DIRECTION('ref_axis',(-1.,0.,0.));
#8550=DIRECTION('center_axis',(0.,0.,1.));
#8551=DIRECTION('ref_axis',(1.,0.,0.));
#8552=DIRECTION('center_axis',(0.,0.,-1.));
#8553=DIRECTION('ref_axis',(-1.,0.,0.));
#8554=DIRECTION('center_axis',(0.,0.,-1.));
#8555=DIRECTION('ref_axis',(-1.,0.,0.));
#8556=DIRECTION('center_axis',(0.,0.,1.));
#8557=DIRECTION('ref_axis',(1.,0.,0.));
#8558=DIRECTION('center_axis',(0.,0.,-1.));
#8559=DIRECTION('ref_axis',(-1.,0.,0.));
#8560=DIRECTION('center_axis',(0.,0.,1.));
#8561=DIRECTION('ref_axis',(1.,0.,0.));
#8562=DIRECTION('center_axis',(0.,0.,-1.));
#8563=DIRECTION('ref_axis',(-1.,0.,0.));
#8564=DIRECTION('center_axis',(0.,0.,-1.));
#8565=DIRECTION('ref_axis',(-1.,0.,0.));
#8566=DIRECTION('center_axis',(1.0701355254071E-15,-1.89923231202752E-15,
1.));
#8567=DIRECTION('ref_axis',(-3.13557062175357E-31,-1.,-1.89923231202752E-15));
#8568=DIRECTION('center_axis',(0.,0.,-1.));
#8569=DIRECTION('ref_axis',(-1.,0.,0.));
#8570=DIRECTION('center_axis',(0.,0.,-1.));
#8571=DIRECTION('ref_axis',(-1.,0.,0.));
#8572=DIRECTION('center_axis',(0.,0.,1.));
#8573=DIRECTION('ref_axis',(1.,0.,0.));
#8574=DIRECTION('center_axis',(-9.64626581390635E-16,9.55613138574038E-16,
-1.));
#8575=DIRECTION('ref_axis',(-1.,-2.27086151733484E-32,9.64626581390635E-16));
#8576=DIRECTION('center_axis',(0.,0.,-1.));
#8577=DIRECTION('ref_axis',(-1.,0.,0.));
#8578=DIRECTION('center_axis',(0.,0.,-1.));
#8579=DIRECTION('ref_axis',(-1.,0.,0.));
#8580=DIRECTION('center_axis',(0.,0.,1.));
#8581=DIRECTION('ref_axis',(1.,0.,0.));
#8582=DIRECTION('center_axis',(-7.44864032782697E-16,1.13528784227057E-15,
-1.));
#8583=DIRECTION('ref_axis',(1.34170956239683E-32,1.,1.13528784227057E-15));
#8584=DIRECTION('center_axis',(0.,0.,-1.));
#8585=DIRECTION('ref_axis',(-1.,0.,0.));
#8586=DIRECTION('center_axis',(0.,0.,-1.));
#8587=DIRECTION('ref_axis',(-1.,0.,0.));
#8588=DIRECTION('center_axis',(-2.50582917348388E-16,-2.16552109648484E-15,
1.));
#8589=DIRECTION('ref_axis',(-6.10963913452999E-32,-1.,-2.16552109648484E-15));
#8590=DIRECTION('center_axis',(0.,0.,-1.));
#8591=DIRECTION('ref_axis',(-1.,0.,0.));
#8592=DIRECTION('center_axis',(1.05120912399335E-15,-8.59453483193718E-16,
-1.));
#8593=DIRECTION('ref_axis',(-1.,6.24131468909447E-33,-1.05120912399335E-15));
#8594=DIRECTION('center_axis',(0.,0.,-1.));
#8595=DIRECTION('ref_axis',(-1.,0.,0.));
#8596=DIRECTION('center_axis',(0.,0.,1.));
#8597=DIRECTION('ref_axis',(1.,0.,0.));
#8598=DIRECTION('center_axis',(-2.18703987820084E-16,1.34010054766509E-15,
-1.));
#8599=DIRECTION('ref_axis',(-2.70980336596201E-33,1.,1.34010054766509E-15));
#8600=DIRECTION('center_axis',(0.,0.,-1.));
#8601=DIRECTION('ref_axis',(-1.,0.,0.));
#8602=DIRECTION('center_axis',(0.,0.,-1.));
#8603=DIRECTION('ref_axis',(-1.,0.,0.));
#8604=DIRECTION('center_axis',(0.,0.,1.));
#8605=DIRECTION('ref_axis',(1.,0.,0.));
#8606=DIRECTION('center_axis',(0.,0.,-1.));
#8607=DIRECTION('ref_axis',(-1.,0.,0.));
#8608=DIRECTION('center_axis',(6.10756095622563E-16,-1.21271509589044E-15,
-1.));
#8609=DIRECTION('ref_axis',(-1.35391388547399E-32,1.,-1.21271509589044E-15));
#8610=DIRECTION('center_axis',(0.,0.,-1.));
#8611=DIRECTION('ref_axis',(-1.,0.,0.));
#8612=DIRECTION('center_axis',(0.,0.,1.));
#8613=DIRECTION('ref_axis',(1.,0.,0.));
#8614=DIRECTION('center_axis',(3.45271963499982E-16,1.31319769393704E-15,
-1.));
#8615=DIRECTION('ref_axis',(-6.73653793160646E-33,1.,1.31319769393704E-15));
#8616=DIRECTION('center_axis',(0.,0.,-1.));
#8617=DIRECTION('ref_axis',(-1.,0.,0.));
#8618=DIRECTION('center_axis',(0.,0.,1.));
#8619=DIRECTION('ref_axis',(1.,0.,0.));
#8620=DIRECTION('center_axis',(0.,0.,-1.));
#8621=DIRECTION('ref_axis',(-1.,0.,0.));
#8622=DIRECTION('center_axis',(0.,0.,-1.));
#8623=DIRECTION('ref_axis',(-1.,0.,0.));
#8624=DIRECTION('center_axis',(6.4697789773697E-17,-1.35628725133693E-15,
-1.));
#8625=DIRECTION('ref_axis',(2.45620303515335E-34,1.,-1.35628725133693E-15));
#8626=DIRECTION('center_axis',(0.,0.,1.));
#8627=DIRECTION('ref_axis',(1.,0.,0.));
#8628=DIRECTION('center_axis',(0.,0.,-1.));
#8629=DIRECTION('ref_axis',(-1.,0.,0.));
#8630=DIRECTION('center_axis',(8.49547255633585E-16,1.05923102890075E-15,
-1.));
#8631=DIRECTION('ref_axis',(-6.4561121370934E-34,1.,1.05923102890075E-15));
#8632=DIRECTION('center_axis',(0.,0.,-1.));
#8633=DIRECTION('ref_axis',(-1.,0.,0.));
#8634=DIRECTION('center_axis',(0.,0.,1.));
#8635=DIRECTION('ref_axis',(1.,0.,0.));
#8636=DIRECTION('center_axis',(0.,0.,-1.));
#8637=DIRECTION('ref_axis',(-1.,0.,0.));
#8638=DIRECTION('center_axis',(0.,0.,-1.));
#8639=DIRECTION('ref_axis',(-1.,0.,0.));
#8640=DIRECTION('center_axis',(-4.92547351688011E-16,-1.26534501954439E-15,
-1.));
#8641=DIRECTION('ref_axis',(1.39597070338681E-32,1.,-1.26534501954439E-15));
#8642=DIRECTION('center_axis',(0.,0.,1.));
#8643=DIRECTION('ref_axis',(1.,0.,0.));
#8644=DIRECTION('center_axis',(0.,0.,-1.));
#8645=DIRECTION('ref_axis',(-1.,0.,0.));
#8646=DIRECTION('center_axis',(0.,0.,-1.));
#8647=DIRECTION('ref_axis',(-1.,0.,0.));
#8648=DIRECTION('center_axis',(-7.44864032782725E-16,-1.13528784227056E-15,
-1.));
#8649=DIRECTION('ref_axis',(-1.3417095623968E-32,1.,-1.13528784227056E-15));
#8650=DIRECTION('center_axis',(0.,0.,1.));
#8651=DIRECTION('ref_axis',(1.,0.,0.));
#8652=DIRECTION('center_axis',(0.,0.,-1.));
#8653=DIRECTION('ref_axis',(-1.,0.,0.));
#8654=DIRECTION('center_axis',(0.,0.,-1.));
#8655=DIRECTION('ref_axis',(-1.,0.,0.));
#8656=DIRECTION('center_axis',(0.,0.,-1.));
#8657=DIRECTION('ref_axis',(-1.,0.,0.));
#8658=DIRECTION('center_axis',(0.,0.,1.));
#8659=DIRECTION('ref_axis',(1.,0.,0.));
#8660=DIRECTION('center_axis',(0.,0.,-1.));
#8661=DIRECTION('ref_axis',(-1.,0.,0.));
#8662=DIRECTION('center_axis',(-1.14223031959991E-15,-7.34173555181192E-16,
-1.));
#8663=DIRECTION('ref_axis',(-1.,1.83215133257436E-32,1.14223031959991E-15));
#8664=DIRECTION('center_axis',(0.,0.,1.));
#8665=DIRECTION('ref_axis',(1.,0.,0.));
#8666=DIRECTION('center_axis',(0.,0.,-1.));
#8667=DIRECTION('ref_axis',(-1.,0.,0.));
#8668=DIRECTION('center_axis',(-4.15432588173314E-15,3.95257705004225E-14,
1.));
#8669=DIRECTION('ref_axis',(1.01104027505707E-32,-1.,3.95257705004225E-14));
#8670=DIRECTION('center_axis',(-1.26991311181345E-15,-4.80647064471381E-16,
-1.));
#8671=DIRECTION('ref_axis',(-1.,-1.14267906456524E-32,1.26991311181345E-15));
#8672=DIRECTION('center_axis',(0.,0.,1.));
#8673=DIRECTION('ref_axis',(1.,0.,0.));
#8674=DIRECTION('center_axis',(0.,0.,-1.));
#8675=DIRECTION('ref_axis',(-1.,0.,0.));
#8676=DIRECTION('center_axis',(0.,0.,1.));
#8677=DIRECTION('ref_axis',(1.,0.,0.));
#8678=DIRECTION('center_axis',(0.,0.,-1.));
#8679=DIRECTION('ref_axis',(-1.,0.,0.));
#8680=DIRECTION('center_axis',(0.,0.,-1.));
#8681=DIRECTION('ref_axis',(-1.,0.,0.));
#8682=DIRECTION('center_axis',(0.,0.,1.));
#8683=DIRECTION('ref_axis',(1.,0.,0.));
#8684=DIRECTION('center_axis',(0.,0.,-1.));
#8685=DIRECTION('ref_axis',(-1.,0.,0.));
#8686=DIRECTION('center_axis',(0.,0.,1.));
#8687=DIRECTION('ref_axis',(1.,0.,0.));
#8688=DIRECTION('center_axis',(0.,0.,-1.));
#8689=DIRECTION('ref_axis',(-1.,0.,0.));
#8690=DIRECTION('center_axis',(-1.35562012840529E-15,7.74272536198692E-17,
-1.));
#8691=DIRECTION('ref_axis',(-1.,-2.42293261278252E-34,1.35562012840529E-15));
#8692=DIRECTION('center_axis',(0.,0.,1.));
#8693=DIRECTION('ref_axis',(1.,0.,0.));
#8694=DIRECTION('center_axis',(0.,0.,-1.));
#8695=DIRECTION('ref_axis',(-1.,0.,0.));
#8696=DIRECTION('center_axis',(0.,0.,1.));
#8697=DIRECTION('ref_axis',(1.,0.,0.));
#8698=DIRECTION('center_axis',(0.,0.,-1.));
#8699=DIRECTION('ref_axis',(-1.,0.,0.));
#8700=DIRECTION('center_axis',(-1.3098985448906E-15,3.57584555363018E-16,
-1.));
#8701=DIRECTION('ref_axis',(-1.,-5.79704190756504E-33,1.3098985448906E-15));
#8702=DIRECTION('center_axis',(0.,0.,1.));
#8703=DIRECTION('ref_axis',(1.,0.,0.));
#8704=DIRECTION('center_axis',(0.,0.,-1.));
#8705=DIRECTION('ref_axis',(-1.,0.,0.));
#8706=DIRECTION('center_axis',(0.,0.,1.));
#8707=DIRECTION('ref_axis',(1.,0.,0.));
#8708=DIRECTION('center_axis',(0.,0.,-1.));
#8709=DIRECTION('ref_axis',(-1.,0.,0.));
#8710=DIRECTION('',(0.,-1.,0.));
#8711=DIRECTION('',(0.,1.,0.));
#8712=DIRECTION('',(-1.,0.,0.));
#8713=DIRECTION('center_axis',(0.,0.,1.));
#8714=DIRECTION('ref_axis',(1.,0.,0.));
#8715=DIRECTION('center_axis',(0.,0.,-1.));
#8716=DIRECTION('ref_axis',(-1.,0.,0.));
#8717=DIRECTION('center_axis',(-7.4486403278271E-16,1.13528784227057E-15,
-1.));
#8718=DIRECTION('ref_axis',(1.34170956239694E-32,1.,1.13528784227057E-15));
#8719=DIRECTION('center_axis',(0.,0.,-1.));
#8720=DIRECTION('ref_axis',(-1.,0.,0.));
#8721=DIRECTION('center_axis',(0.,0.,-1.));
#8722=DIRECTION('ref_axis',(-1.,0.,0.));
#8723=DIRECTION('center_axis',(0.,0.,-1.));
#8724=DIRECTION('ref_axis',(-1.,0.,0.));
#8725=DIRECTION('center_axis',(0.,0.,-1.));
#8726=DIRECTION('ref_axis',(-1.,0.,0.));
#8727=DIRECTION('center_axis',(0.,0.,-1.));
#8728=DIRECTION('ref_axis',(-1.,0.,0.));
#8729=DIRECTION('center_axis',(0.,0.,-1.));
#8730=DIRECTION('ref_axis',(-1.,0.,0.));
#8731=DIRECTION('center_axis',(0.,0.,-1.));
#8732=DIRECTION('ref_axis',(-1.,0.,0.));
#8733=DIRECTION('center_axis',(0.,0.,-1.));
#8734=DIRECTION('ref_axis',(-1.,0.,0.));
#8735=DIRECTION('center_axis',(1.35562012840529E-15,-7.74272536198712E-17,
-1.));
#8736=DIRECTION('ref_axis',(-1.,-2.42293261278146E-34,-1.35562012840529E-15));
#8737=DIRECTION('center_axis',(-1.1422303195999E-15,7.34173555181211E-16,
-1.));
#8738=DIRECTION('ref_axis',(-1.,-1.83215133257424E-32,1.1422303195999E-15));
#8739=DIRECTION('center_axis',(0.,0.,-1.));
#8740=DIRECTION('ref_axis',(-1.,0.,0.));
#8741=DIRECTION('center_axis',(0.,0.,-1.));
#8742=DIRECTION('ref_axis',(-1.,0.,0.));
#8743=DIRECTION('center_axis',(0.,0.,-1.));
#8744=DIRECTION('ref_axis',(-1.,0.,0.));
#8745=DIRECTION('center_axis',(1.34209460732158E-15,2.0611399064365E-16,
-1.));
#8746=DIRECTION('ref_axis',(-1.,-2.1428061985013E-33,-1.34209460732158E-15));
#8747=DIRECTION('center_axis',(0.,0.,-1.));
#8748=DIRECTION('ref_axis',(-1.,0.,0.));
#8749=DIRECTION('center_axis',(0.,0.,-1.));
#8750=DIRECTION('ref_axis',(-1.,0.,0.));
#8751=DIRECTION('center_axis',(0.,0.,-1.));
#8752=DIRECTION('ref_axis',(-1.,0.,0.));
#8753=DIRECTION('center_axis',(0.,0.,-1.));
#8754=DIRECTION('ref_axis',(-1.,0.,0.));
#8755=DIRECTION('center_axis',(0.,0.,-1.));
#8756=DIRECTION('ref_axis',(-1.,0.,0.));
#8757=DIRECTION('center_axis',(4.15432588173204E-15,-3.95257705004099E-14,
1.));
#8758=DIRECTION('ref_axis',(1.011040284911E-32,-1.,-3.95257705004099E-14));
#8759=DIRECTION('center_axis',(0.,0.,-1.));
#8760=DIRECTION('ref_axis',(-1.,0.,0.));
#8761=DIRECTION('center_axis',(0.,0.,-1.));
#8762=DIRECTION('ref_axis',(-1.,0.,0.));
#8763=DIRECTION('center_axis',(0.,0.,-1.));
#8764=DIRECTION('ref_axis',(-1.,0.,0.));
#8765=DIRECTION('center_axis',(0.,0.,-1.));
#8766=DIRECTION('ref_axis',(-1.,0.,0.));
#8767=DIRECTION('center_axis',(0.,0.,-1.));
#8768=DIRECTION('ref_axis',(-1.,0.,0.));
#8769=DIRECTION('center_axis',(0.,0.,-1.));
#8770=DIRECTION('ref_axis',(-1.,0.,0.));
#8771=DIRECTION('center_axis',(0.,0.,-1.));
#8772=DIRECTION('ref_axis',(-1.,0.,0.));
#8773=DIRECTION('center_axis',(0.,0.,-1.));
#8774=DIRECTION('ref_axis',(-1.,0.,0.));
#8775=DIRECTION('center_axis',(0.,0.,-1.));
#8776=DIRECTION('ref_axis',(-1.,0.,0.));
#8777=DIRECTION('center_axis',(7.44864032782723E-16,1.13528784227056E-15,
-1.));
#8778=DIRECTION('ref_axis',(-1.34170956239609E-32,1.,1.13528784227056E-15));
#8779=DIRECTION('center_axis',(0.,0.,-1.));
#8780=DIRECTION('ref_axis',(-1.,0.,0.));
#8781=DIRECTION('center_axis',(0.,0.,-1.));
#8782=DIRECTION('ref_axis',(-1.,0.,0.));
#8783=DIRECTION('center_axis',(0.,0.,-1.));
#8784=DIRECTION('ref_axis',(-1.,0.,0.));
#8785=DIRECTION('center_axis',(0.,0.,-1.));
#8786=DIRECTION('ref_axis',(-1.,0.,0.));
#8787=DIRECTION('center_axis',(0.,0.,-1.));
#8788=DIRECTION('ref_axis',(-1.,0.,0.));
#8789=DIRECTION('center_axis',(0.,0.,-1.));
#8790=DIRECTION('ref_axis',(-1.,0.,0.));
#8791=DIRECTION('center_axis',(0.,0.,-1.));
#8792=DIRECTION('ref_axis',(-1.,0.,0.));
#8793=DIRECTION('center_axis',(0.,0.,-1.));
#8794=DIRECTION('ref_axis',(-1.,0.,0.));
#8795=DIRECTION('center_axis',(0.,0.,-1.));
#8796=DIRECTION('ref_axis',(-1.,0.,0.));
#8797=DIRECTION('center_axis',(0.,0.,-1.));
#8798=DIRECTION('ref_axis',(-1.,0.,0.));
#8799=DIRECTION('center_axis',(0.,0.,-1.));
#8800=DIRECTION('ref_axis',(-1.,0.,0.));
#8801=DIRECTION('center_axis',(-6.46977897736951E-17,1.35628725133693E-15,
-1.));
#8802=DIRECTION('ref_axis',(2.4562030351539E-34,1.,1.35628725133693E-15));
#8803=DIRECTION('center_axis',(-6.10756095622592E-16,-1.21271509589044E-15,
-1.));
#8804=DIRECTION('ref_axis',(1.35391388547316E-32,1.,-1.21271509589044E-15));
#8805=DIRECTION('center_axis',(0.,0.,-1.));
#8806=DIRECTION('ref_axis',(-1.,0.,0.));
#8807=DIRECTION('center_axis',(0.,0.,-1.));
#8808=DIRECTION('ref_axis',(-1.,0.,0.));
#8809=DIRECTION('center_axis',(0.,0.,-1.));
#8810=DIRECTION('ref_axis',(-1.,0.,0.));
#8811=DIRECTION('center_axis',(-3.45271963499982E-16,-1.31319769393704E-15,
-1.));
#8812=DIRECTION('ref_axis',(-6.73653793160646E-33,1.,-1.31319769393704E-15));
#8813=DIRECTION('center_axis',(0.,0.,-1.));
#8814=DIRECTION('ref_axis',(-1.,0.,0.));
#8815=DIRECTION('center_axis',(0.,0.,-1.));
#8816=DIRECTION('ref_axis',(-1.,0.,0.));
#8817=DIRECTION('center_axis',(0.,0.,-1.));
#8818=DIRECTION('ref_axis',(-1.,0.,0.));
#8819=DIRECTION('center_axis',(-6.46977897737243E-17,-1.35628725133692E-15,
-1.));
#8820=DIRECTION('ref_axis',(-2.45620303514865E-34,1.,-1.35628725133692E-15));
#8821=DIRECTION('center_axis',(0.,0.,-1.));
#8822=DIRECTION('ref_axis',(-1.,0.,0.));
#8823=DIRECTION('center_axis',(0.,0.,-1.));
#8824=DIRECTION('ref_axis',(-1.,0.,0.));
#8825=DIRECTION('center_axis',(0.,0.,-1.));
#8826=DIRECTION('ref_axis',(-1.,0.,0.));
#8827=DIRECTION('center_axis',(2.18703987820084E-16,-1.34010054766509E-15,
-1.));
#8828=DIRECTION('ref_axis',(-2.70980336596175E-33,1.,-1.34010054766509E-15));
#8829=DIRECTION('center_axis',(0.,0.,-1.));
#8830=DIRECTION('ref_axis',(-1.,0.,0.));
#8831=DIRECTION('center_axis',(0.,0.,-1.));
#8832=DIRECTION('ref_axis',(-1.,0.,0.));
#8833=DIRECTION('center_axis',(0.,0.,-1.));
#8834=DIRECTION('ref_axis',(-1.,0.,0.));
#8835=DIRECTION('center_axis',(4.92547351687991E-16,-1.26534501954442E-15,
-1.));
#8836=DIRECTION('ref_axis',(-1.39597070338527E-32,1.,-1.26534501954442E-15));
#8837=DIRECTION('center_axis',(-2.50582917348388E-16,-2.16552109648484E-15,
-1.));
#8838=DIRECTION('ref_axis',(6.10963913452999E-32,1.,-2.16552109648484E-15));
#8839=DIRECTION('center_axis',(0.,0.,-1.));
#8840=DIRECTION('ref_axis',(-1.,0.,0.));
#8841=DIRECTION('center_axis',(-1.2069281093736E-15,6.22113696155734E-16,
-1.));
#8842=DIRECTION('ref_axis',(-1.,1.73910758130861E-32,1.2069281093736E-15));
#8843=DIRECTION('center_axis',(7.44864032782693E-16,-1.13528784227057E-15,
-1.));
#8844=DIRECTION('ref_axis',(1.34170956239657E-32,1.,-1.13528784227057E-15));
#8845=DIRECTION('center_axis',(0.,0.,-1.));
#8846=DIRECTION('ref_axis',(-1.,0.,0.));
#8847=DIRECTION('center_axis',(0.,0.,-1.));
#8848=DIRECTION('ref_axis',(-1.,0.,0.));
#8849=DIRECTION('center_axis',(0.,0.,-1.));
#8850=DIRECTION('ref_axis',(-1.,0.,0.));
#8851=DIRECTION('center_axis',(0.,0.,-1.));
#8852=DIRECTION('ref_axis',(-1.,0.,0.));
#8853=DIRECTION('center_axis',(0.,0.,-1.));
#8854=DIRECTION('ref_axis',(-1.,0.,0.));
#8855=DIRECTION('center_axis',(0.,0.,-1.));
#8856=DIRECTION('ref_axis',(-1.,0.,0.));
#8857=DIRECTION('center_axis',(0.,0.,-1.));
#8858=DIRECTION('ref_axis',(-1.,0.,0.));
#8859=DIRECTION('center_axis',(1.0701355254071E-15,-1.89923231202752E-15,
-1.));
#8860=DIRECTION('ref_axis',(3.13557062175357E-31,1.,-1.89923231202752E-15));
#8861=DIRECTION('center_axis',(0.,0.,-1.));
#8862=DIRECTION('ref_axis',(-1.,0.,0.));
#8863=DIRECTION('center_axis',(1.26991311181345E-15,-4.80647064471377E-16,
-1.));
#8864=DIRECTION('ref_axis',(-1.,1.14267906456546E-32,-1.26991311181345E-15));
#8865=DIRECTION('center_axis',(0.,0.,-1.));
#8866=DIRECTION('ref_axis',(-1.,0.,0.));
#8867=DIRECTION('center_axis',(0.,0.,-1.));
#8868=DIRECTION('ref_axis',(-1.,0.,0.));
#8869=DIRECTION('center_axis',(0.,0.,-1.));
#8870=DIRECTION('ref_axis',(-1.,0.,0.));
#8871=DIRECTION('center_axis',(0.,0.,-1.));
#8872=DIRECTION('ref_axis',(-1.,0.,0.));
#8873=DIRECTION('center_axis',(0.,0.,-1.));
#8874=DIRECTION('ref_axis',(-1.,0.,0.));
#8875=DIRECTION('center_axis',(0.,0.,-1.));
#8876=DIRECTION('ref_axis',(-1.,0.,0.));
#8877=DIRECTION('center_axis',(0.,0.,-1.));
#8878=DIRECTION('ref_axis',(-1.,0.,0.));
#8879=DIRECTION('center_axis',(0.,0.,-1.));
#8880=DIRECTION('ref_axis',(-1.,0.,0.));
#8881=DIRECTION('center_axis',(0.,0.,-1.));
#8882=DIRECTION('ref_axis',(-1.,0.,0.));
#8883=DIRECTION('center_axis',(1.35562012840529E-15,7.74272536198596E-17,
-1.));
#8884=DIRECTION('ref_axis',(-1.,2.42293261278592E-34,-1.35562012840529E-15));
#8885=DIRECTION('center_axis',(0.,0.,-1.));
#8886=DIRECTION('ref_axis',(-1.,0.,0.));
#8887=DIRECTION('center_axis',(0.,0.,-1.));
#8888=DIRECTION('ref_axis',(-1.,0.,0.));
#8889=DIRECTION('center_axis',(0.,0.,-1.));
#8890=DIRECTION('ref_axis',(-1.,0.,0.));
#8891=DIRECTION('center_axis',(0.,0.,-1.));
#8892=DIRECTION('ref_axis',(-1.,0.,0.));
#8893=DIRECTION('center_axis',(1.3098985448906E-15,3.57584555363002E-16,
-1.));
#8894=DIRECTION('ref_axis',(-1.,5.79704190755911E-33,-1.3098985448906E-15));
#8895=DIRECTION('center_axis',(0.,0.,-1.));
#8896=DIRECTION('ref_axis',(-1.,0.,0.));
#8897=DIRECTION('center_axis',(0.,0.,-1.));
#8898=DIRECTION('ref_axis',(-1.,0.,0.));
#8899=DIRECTION('center_axis',(0.,0.,-1.));
#8900=DIRECTION('ref_axis',(-1.,0.,0.));
#8901=DIRECTION('center_axis',(0.,0.,-1.));
#8902=DIRECTION('ref_axis',(-1.,0.,0.));
#8903=DIRECTION('center_axis',(1.2069281093736E-15,6.22113696155711E-16,
-1.));
#8904=DIRECTION('ref_axis',(-1.,-1.73910758130838E-32,-1.2069281093736E-15));
#8905=DIRECTION('center_axis',(0.,0.,-1.));
#8906=DIRECTION('ref_axis',(-1.,0.,0.));
#8907=DIRECTION('center_axis',(0.,0.,-1.));
#8908=DIRECTION('ref_axis',(-1.,0.,0.));
#8909=DIRECTION('center_axis',(2.50582917348385E-16,-2.16552109648485E-15,
-1.));
#8910=DIRECTION('ref_axis',(-6.10963913452889E-32,1.,-2.16552109648485E-15));
#8911=DIRECTION('center_axis',(0.,0.,-1.));
#8912=DIRECTION('ref_axis',(-1.,0.,0.));
#8913=DIRECTION('center_axis',(0.,0.,-1.));
#8914=DIRECTION('ref_axis',(-1.,0.,0.));
#8915=DIRECTION('center_axis',(0.,0.,-1.));
#8916=DIRECTION('ref_axis',(-1.,0.,0.));
#8917=DIRECTION('center_axis',(0.,0.,-1.));
#8918=DIRECTION('ref_axis',(-1.,0.,0.));
#8919=DIRECTION('center_axis',(0.,0.,-1.));
#8920=DIRECTION('ref_axis',(-1.,0.,0.));
#8921=DIRECTION('center_axis',(0.,0.,-1.));
#8922=DIRECTION('ref_axis',(-1.,0.,0.));
#8923=DIRECTION('center_axis',(0.,0.,-1.));
#8924=DIRECTION('ref_axis',(-1.,0.,0.));
#8925=DIRECTION('center_axis',(0.,0.,-1.));
#8926=DIRECTION('ref_axis',(-1.,0.,0.));
#8927=DIRECTION('center_axis',(0.,0.,-1.));
#8928=DIRECTION('ref_axis',(-1.,0.,0.));
#8929=DIRECTION('center_axis',(0.,0.,-1.));
#8930=DIRECTION('ref_axis',(-1.,0.,0.));
#8931=DIRECTION('center_axis',(0.,0.,-1.));
#8932=DIRECTION('ref_axis',(-1.,0.,0.));
#8933=DIRECTION('center_axis',(6.10756095622582E-16,1.21271509589044E-15,
-1.));
#8934=DIRECTION('ref_axis',(1.35391388547304E-32,1.,1.21271509589044E-15));
#8935=DIRECTION('center_axis',(0.,0.,-1.));
#8936=DIRECTION('ref_axis',(-1.,0.,0.));
#8937=DIRECTION('center_axis',(0.,0.,-1.));
#8938=DIRECTION('ref_axis',(-1.,0.,0.));
#8939=DIRECTION('center_axis',(0.,0.,-1.));
#8940=DIRECTION('ref_axis',(-1.,0.,0.));
#8941=DIRECTION('center_axis',(0.,0.,-1.));
#8942=DIRECTION('ref_axis',(-1.,0.,0.));
#8943=DIRECTION('center_axis',(0.,0.,-1.));
#8944=DIRECTION('ref_axis',(-1.,0.,0.));
#8945=DIRECTION('center_axis',(1.47558720267693E-15,1.6046544254399E-15,
-1.));
#8946=DIRECTION('ref_axis',(2.31817004142331E-33,1.,1.6046544254399E-15));
#8947=DIRECTION('center_axis',(0.,0.,-1.));
#8948=DIRECTION('ref_axis',(-1.,0.,0.));
#8949=DIRECTION('center_axis',(1.77696849674338E-15,-1.26279704599333E-15,
-1.));
#8950=DIRECTION('ref_axis',(-1.,-2.1561382677115E-31,-1.77696849674338E-15));
#8951=DIRECTION('center_axis',(0.,0.,-1.));
#8952=DIRECTION('ref_axis',(-1.,0.,0.));
#8953=DIRECTION('center_axis',(6.46977897737148E-17,1.35628725133693E-15,
-1.));
#8954=DIRECTION('ref_axis',(-2.45620303515642E-34,1.,1.35628725133693E-15));
#8955=DIRECTION('center_axis',(0.,0.,-1.));
#8956=DIRECTION('ref_axis',(-1.,0.,0.));
#8957=DIRECTION('center_axis',(0.,0.,-1.));
#8958=DIRECTION('ref_axis',(-1.,0.,0.));
#8959=DIRECTION('center_axis',(0.,0.,-1.));
#8960=DIRECTION('ref_axis',(-1.,0.,0.));
#8961=DIRECTION('center_axis',(0.,0.,-1.));
#8962=DIRECTION('ref_axis',(-1.,0.,0.));
#8963=DIRECTION('center_axis',(-2.18703987820093E-16,1.34010054766509E-15,
-1.));
#8964=DIRECTION('ref_axis',(-2.70980336596394E-33,1.,1.34010054766509E-15));
#8965=DIRECTION('center_axis',(0.,0.,-1.));
#8966=DIRECTION('ref_axis',(-1.,0.,0.));
#8967=DIRECTION('center_axis',(0.,0.,-1.));
#8968=DIRECTION('ref_axis',(-1.,0.,0.));
#8969=DIRECTION('center_axis',(0.,0.,-1.));
#8970=DIRECTION('ref_axis',(-1.,0.,0.));
#8971=DIRECTION('center_axis',(0.,0.,-1.));
#8972=DIRECTION('ref_axis',(-1.,0.,0.));
#8973=DIRECTION('center_axis',(0.,0.,-1.));
#8974=DIRECTION('ref_axis',(-1.,0.,0.));
#8975=DIRECTION('center_axis',(0.,0.,-1.));
#8976=DIRECTION('ref_axis',(-1.,0.,0.));
#8977=DIRECTION('center_axis',(0.,0.,-1.));
#8978=DIRECTION('ref_axis',(-1.,0.,0.));
#8979=DIRECTION('center_axis',(2.17985119260763E-15,2.28516055189852E-17,
-1.));
#8980=DIRECTION('ref_axis',(-1.,-5.24414567525364E-33,-2.17985119260763E-15));
#8981=DIRECTION('',(0.,-1.,0.));
#8982=DIRECTION('',(-1.,0.,0.));
#8983=DIRECTION('',(0.,1.,0.));
#8984=DIRECTION('center_axis',(0.,0.,-1.));
#8985=DIRECTION('ref_axis',(-1.,0.,0.));
#8986=DIRECTION('',(0.,0.,-1.));
#8987=DIRECTION('center_axis',(0.,0.,1.));
#8988=DIRECTION('ref_axis',(1.,0.,0.));
#8989=DIRECTION('',(0.,0.,1.));
#8990=DIRECTION('center_axis',(0.,0.,1.));
#8991=DIRECTION('ref_axis',(1.,0.,0.));
#8992=DIRECTION('',(0.,0.,-1.));
#8993=DIRECTION('center_axis',(0.,0.,1.));
#8994=DIRECTION('ref_axis',(1.,0.,0.));
#8995=DIRECTION('',(0.,0.,-1.));
#8996=DIRECTION('',(0.,0.,1.));
#8997=DIRECTION('center_axis',(0.,0.,-1.));
#8998=DIRECTION('ref_axis',(-1.,0.,0.));
#8999=DIRECTION('center_axis',(0.,0.,-1.));
#9000=DIRECTION('ref_axis',(-1.,0.,0.));
#9001=DIRECTION('center_axis',(0.,0.,1.));
#9002=DIRECTION('ref_axis',(-0.988411742041742,-0.151796667269113,0.));
#9003=DIRECTION('',(0.,0.,-1.));
#9004=DIRECTION('center_axis',(0.,0.,1.));
#9005=DIRECTION('ref_axis',(1.,0.,0.));
#9006=DIRECTION('',(0.,0.,1.));
#9007=DIRECTION('center_axis',(0.,0.,-1.));
#9008=DIRECTION('ref_axis',(-1.,0.,0.));
#9009=DIRECTION('',(0.,0.,-1.));
#9010=DIRECTION('center_axis',(0.,0.,1.));
#9011=DIRECTION('ref_axis',(1.,0.,0.));
#9012=DIRECTION('',(0.,0.,1.));
#9013=DIRECTION('center_axis',(0.,0.,-1.));
#9014=DIRECTION('ref_axis',(0.802811069346196,0.596233500346314,0.));
#9015=DIRECTION('center_axis',(0.,0.,1.));
#9016=DIRECTION('ref_axis',(1.,0.,0.));
#9017=DIRECTION('center_axis',(0.,0.,1.));
#9018=DIRECTION('ref_axis',(1.,0.,0.));
#9019=DIRECTION('',(0.,0.,1.));
#9020=DIRECTION('center_axis',(0.,0.,-1.));
#9021=DIRECTION('ref_axis',(-1.,0.,0.));
#9022=DIRECTION('',(0.,0.,-1.));
#9023=DIRECTION('center_axis',(0.,0.,1.));
#9024=DIRECTION('ref_axis',(1.,0.,0.));
#9025=DIRECTION('center_axis',(0.,0.,1.));
#9026=DIRECTION('ref_axis',(1.,0.,0.));
#9027=DIRECTION('center_axis',(0.,0.,1.));
#9028=DIRECTION('ref_axis',(1.,0.,0.));
#9029=DIRECTION('',(0.,0.,1.));
#9030=DIRECTION('center_axis',(0.,0.,-1.));
#9031=DIRECTION('ref_axis',(-1.,0.,0.));
#9032=DIRECTION('',(0.,0.,-1.));
#9033=DIRECTION('center_axis',(0.,0.,1.));
#9034=DIRECTION('ref_axis',(1.,0.,0.));
#9035=DIRECTION('center_axis',(0.,0.,1.));
#9036=DIRECTION('ref_axis',(1.,0.,0.));
#9037=DIRECTION('center_axis',(0.,0.,1.));
#9038=DIRECTION('ref_axis',(1.,0.,0.));
#9039=DIRECTION('',(0.,0.,1.));
#9040=DIRECTION('center_axis',(0.,0.,-1.));
#9041=DIRECTION('ref_axis',(-1.,0.,0.));
#9042=DIRECTION('',(0.,0.,-1.));
#9043=DIRECTION('center_axis',(0.,0.,1.));
#9044=DIRECTION('ref_axis',(1.,0.,0.));
#9045=DIRECTION('center_axis',(0.,0.,1.));
#9046=DIRECTION('ref_axis',(1.,0.,0.));
#9047=DIRECTION('center_axis',(0.,0.,1.));
#9048=DIRECTION('ref_axis',(1.,0.,0.));
#9049=DIRECTION('',(0.,0.,1.));
#9050=DIRECTION('center_axis',(0.,0.,-1.));
#9051=DIRECTION('ref_axis',(-1.,0.,0.));
#9052=DIRECTION('',(0.,0.,-1.));
#9053=DIRECTION('center_axis',(0.,0.,1.));
#9054=DIRECTION('ref_axis',(1.,0.,0.));
#9055=DIRECTION('center_axis',(0.,0.,1.));
#9056=DIRECTION('ref_axis',(1.,0.,0.));
#9057=DIRECTION('center_axis',(0.,0.,1.));
#9058=DIRECTION('ref_axis',(1.,0.,0.));
#9059=DIRECTION('',(0.,0.,1.));
#9060=DIRECTION('center_axis',(0.,0.,-1.));
#9061=DIRECTION('ref_axis',(-1.,0.,0.));
#9062=DIRECTION('',(0.,0.,-1.));
#9063=DIRECTION('center_axis',(0.,0.,1.));
#9064=DIRECTION('ref_axis',(1.,0.,0.));
#9065=DIRECTION('center_axis',(0.,0.,1.));
#9066=DIRECTION('ref_axis',(1.,0.,0.));
#9067=DIRECTION('',(0.,0.,-1.));
#9068=DIRECTION('center_axis',(0.,0.,1.));
#9069=DIRECTION('ref_axis',(1.,0.,0.));
#9070=DIRECTION('center_axis',(0.,0.,1.));
#9071=DIRECTION('ref_axis',(1.,0.,0.));
#9072=DIRECTION('',(0.,0.,1.));
#9073=DIRECTION('center_axis',(0.,0.,-1.));
#9074=DIRECTION('ref_axis',(-1.,0.,0.));
#9075=DIRECTION('center_axis',(0.,0.,1.));
#9076=DIRECTION('ref_axis',(1.,0.,0.));
#9077=DIRECTION('',(0.,0.,-1.));
#9078=DIRECTION('center_axis',(0.,0.,1.));
#9079=DIRECTION('ref_axis',(1.,0.,0.));
#9080=DIRECTION('center_axis',(0.,0.,1.));
#9081=DIRECTION('ref_axis',(1.,0.,0.));
#9082=DIRECTION('',(0.,0.,1.));
#9083=DIRECTION('center_axis',(0.,0.,-1.));
#9084=DIRECTION('ref_axis',(-1.,0.,0.));
#9085=DIRECTION('center_axis',(0.,0.,1.));
#9086=DIRECTION('ref_axis',(1.,0.,0.));
#9087=DIRECTION('',(0.,0.,-1.));
#9088=DIRECTION('center_axis',(0.,0.,1.));
#9089=DIRECTION('ref_axis',(1.,0.,0.));
#9090=DIRECTION('center_axis',(0.,0.,1.));
#9091=DIRECTION('ref_axis',(1.,0.,0.));
#9092=DIRECTION('',(0.,0.,1.));
#9093=DIRECTION('center_axis',(0.,0.,-1.));
#9094=DIRECTION('ref_axis',(-1.,0.,0.));
#9095=DIRECTION('center_axis',(0.,0.,1.));
#9096=DIRECTION('ref_axis',(1.,0.,0.));
#9097=DIRECTION('',(0.,0.,-1.));
#9098=DIRECTION('center_axis',(0.,0.,1.));
#9099=DIRECTION('ref_axis',(1.,0.,0.));
#9100=DIRECTION('center_axis',(0.,0.,1.));
#9101=DIRECTION('ref_axis',(1.,0.,0.));
#9102=DIRECTION('',(0.,0.,1.));
#9103=DIRECTION('center_axis',(0.,0.,-1.));
#9104=DIRECTION('ref_axis',(-1.,0.,0.));
#9105=DIRECTION('center_axis',(0.,0.,1.));
#9106=DIRECTION('ref_axis',(1.,0.,0.));
#9107=DIRECTION('',(0.,0.,-1.));
#9108=DIRECTION('center_axis',(0.,0.,1.));
#9109=DIRECTION('ref_axis',(1.,0.,0.));
#9110=DIRECTION('center_axis',(0.,0.,1.));
#9111=DIRECTION('ref_axis',(1.,0.,0.));
#9112=DIRECTION('',(0.,0.,1.));
#9113=DIRECTION('center_axis',(0.,0.,-1.));
#9114=DIRECTION('ref_axis',(-1.,0.,0.));
#9115=DIRECTION('center_axis',(0.,0.,1.));
#9116=DIRECTION('ref_axis',(1.,0.,0.));
#9117=DIRECTION('',(0.,0.,-1.));
#9118=DIRECTION('center_axis',(0.,0.,1.));
#9119=DIRECTION('ref_axis',(1.,0.,0.));
#9120=DIRECTION('',(0.,0.,1.));
#9121=DIRECTION('center_axis',(0.,0.,-1.));
#9122=DIRECTION('ref_axis',(-1.,0.,0.));
#9123=DIRECTION('center_axis',(0.,0.,1.));
#9124=DIRECTION('ref_axis',(1.,0.,0.));
#9125=DIRECTION('',(0.,0.,-1.));
#9126=DIRECTION('center_axis',(0.,0.,1.));
#9127=DIRECTION('ref_axis',(1.,0.,0.));
#9128=DIRECTION('',(0.,0.,1.));
#9129=DIRECTION('center_axis',(0.,0.,-1.));
#9130=DIRECTION('ref_axis',(-1.,0.,0.));
#9131=DIRECTION('center_axis',(0.,0.,1.));
#9132=DIRECTION('ref_axis',(1.,0.,0.));
#9133=DIRECTION('',(0.,0.,1.));
#9134=DIRECTION('center_axis',(0.,0.,-1.));
#9135=DIRECTION('ref_axis',(-1.,0.,0.));
#9136=DIRECTION('',(0.,0.,-1.));
#9137=DIRECTION('center_axis',(0.,0.,1.));
#9138=DIRECTION('ref_axis',(1.,0.,0.));
#9139=DIRECTION('center_axis',(0.,0.,1.));
#9140=DIRECTION('ref_axis',(1.,0.,0.));
#9141=DIRECTION('',(0.,0.,1.));
#9142=DIRECTION('center_axis',(0.,0.,-1.));
#9143=DIRECTION('ref_axis',(-1.,0.,0.));
#9144=DIRECTION('',(0.,0.,-1.));
#9145=DIRECTION('center_axis',(0.,0.,1.));
#9146=DIRECTION('ref_axis',(1.,0.,0.));
#9147=DIRECTION('center_axis',(0.,0.,1.));
#9148=DIRECTION('ref_axis',(1.,0.,0.));
#9149=DIRECTION('',(0.,0.,-1.));
#9150=DIRECTION('center_axis',(0.,0.,1.));
#9151=DIRECTION('ref_axis',(1.,0.,0.));
#9152=DIRECTION('',(0.,0.,1.));
#9153=DIRECTION('center_axis',(0.,0.,-1.));
#9154=DIRECTION('ref_axis',(-1.,0.,0.));
#9155=DIRECTION('',(0.,0.,-1.));
#9156=DIRECTION('center_axis',(0.,0.,1.));
#9157=DIRECTION('ref_axis',(1.,0.,0.));
#9158=DIRECTION('',(0.,0.,1.));
#9159=DIRECTION('center_axis',(0.,0.,-1.));
#9160=DIRECTION('ref_axis',(-1.,0.,0.));
#9161=DIRECTION('center_axis',(0.,0.,1.));
#9162=DIRECTION('ref_axis',(1.,0.,0.));
#9163=DIRECTION('',(0.,0.,-1.));
#9164=DIRECTION('center_axis',(0.,0.,1.));
#9165=DIRECTION('ref_axis',(-0.98841174204174,0.15179666726912,0.));
#9166=DIRECTION('',(0.,0.,1.));
#9167=DIRECTION('center_axis',(0.,0.,-1.));
#9168=DIRECTION('ref_axis',(0.802811069346189,-0.596233500346323,0.));
#9169=DIRECTION('',(0.,0.,-1.));
#9170=DIRECTION('center_axis',(0.,0.,1.));
#9171=DIRECTION('ref_axis',(1.,0.,0.));
#9172=DIRECTION('',(0.,0.,1.));
#9173=DIRECTION('center_axis',(0.,0.,-1.));
#9174=DIRECTION('ref_axis',(-1.,0.,0.));
#9175=DIRECTION('center_axis',(0.,0.,1.));
#9176=DIRECTION('ref_axis',(1.,0.,0.));
#9177=DIRECTION('',(0.,0.,-1.));
#9178=DIRECTION('center_axis',(0.,0.,1.));
#9179=DIRECTION('ref_axis',(1.,0.,0.));
#9180=DIRECTION('',(0.,0.,1.));
#9181=DIRECTION('center_axis',(0.,0.,-1.));
#9182=DIRECTION('ref_axis',(0.999945056799679,-0.0104825274569905,0.));
#9183=DIRECTION('',(0.,0.,-1.));
#9184=DIRECTION('center_axis',(0.,0.,1.));
#9185=DIRECTION('ref_axis',(1.,0.,0.));
#9186=DIRECTION('',(0.,0.,1.));
#9187=DIRECTION('center_axis',(0.,0.,-1.));
#9188=DIRECTION('ref_axis',(-1.,0.,0.));
#9189=DIRECTION('center_axis',(0.,0.,1.));
#9190=DIRECTION('ref_axis',(1.,0.,0.));
#9191=DIRECTION('',(0.,0.,-1.));
#9192=DIRECTION('center_axis',(0.,0.,1.));
#9193=DIRECTION('ref_axis',(1.,0.,0.));
#9194=DIRECTION('',(0.,0.,1.));
#9195=DIRECTION('center_axis',(0.,0.,-1.));
#9196=DIRECTION('ref_axis',(0.980273298181861,0.197646808402403,0.));
#9197=DIRECTION('',(0.,0.,-1.));
#9198=DIRECTION('center_axis',(0.,0.,1.));
#9199=DIRECTION('ref_axis',(1.,0.,0.));
#9200=DIRECTION('',(0.,0.,1.));
#9201=DIRECTION('center_axis',(0.,0.,-1.));
#9202=DIRECTION('ref_axis',(-1.,0.,0.));
#9203=DIRECTION('center_axis',(0.,0.,1.));
#9204=DIRECTION('ref_axis',(1.,0.,0.));
#9205=DIRECTION('',(0.,0.,-1.));
#9206=DIRECTION('center_axis',(0.,0.,1.));
#9207=DIRECTION('ref_axis',(1.,0.,0.));
#9208=DIRECTION('',(0.,0.,1.));
#9209=DIRECTION('center_axis',(0.,0.,-1.));
#9210=DIRECTION('ref_axis',(0.975914418166608,-0.218153726565764,0.));
#9211=DIRECTION('',(0.,0.,-1.));
#9212=DIRECTION('center_axis',(0.,0.,1.));
#9213=DIRECTION('ref_axis',(1.,0.,0.));
#9214=DIRECTION('',(0.,0.,1.));
#9215=DIRECTION('center_axis',(0.,0.,-1.));
#9216=DIRECTION('ref_axis',(-1.,0.,0.));
#9217=DIRECTION('center_axis',(0.,0.,1.));
#9218=DIRECTION('ref_axis',(1.,0.,0.));
#9219=DIRECTION('',(0.,0.,-1.));
#9220=DIRECTION('center_axis',(0.,0.,1.));
#9221=DIRECTION('ref_axis',(-0.998372875767673,-0.0570228106233482,0.));
#9222=DIRECTION('',(0.,0.,1.));
#9223=DIRECTION('center_axis',(0.,0.,-1.));
#9224=DIRECTION('ref_axis',(0.909231636502712,-0.416290561005893,0.));
#9225=DIRECTION('',(0.,0.,-1.));
#9226=DIRECTION('center_axis',(0.,0.,1.));
#9227=DIRECTION('ref_axis',(1.,0.,0.));
#9228=DIRECTION('',(0.,0.,1.));
#9229=DIRECTION('center_axis',(0.,0.,-1.));
#9230=DIRECTION('ref_axis',(-1.,0.,0.));
#9231=DIRECTION('center_axis',(0.,0.,1.));
#9232=DIRECTION('ref_axis',(1.,0.,0.));
#9233=DIRECTION('',(0.,0.,-1.));
#9234=DIRECTION('center_axis',(0.,0.,1.));
#9235=DIRECTION('ref_axis',(1.,0.,0.));
#9236=DIRECTION('',(0.,0.,1.));
#9237=DIRECTION('center_axis',(0.,0.,-1.));
#9238=DIRECTION('ref_axis',(0.917758892560324,0.397138030319997,0.));
#9239=DIRECTION('',(0.,0.,-1.));
#9240=DIRECTION('center_axis',(0.,0.,1.));
#9241=DIRECTION('ref_axis',(1.,0.,0.));
#9242=DIRECTION('',(0.,0.,1.));
#9243=DIRECTION('center_axis',(0.,0.,-1.));
#9244=DIRECTION('ref_axis',(-1.,0.,0.));
#9245=DIRECTION('center_axis',(0.,0.,1.));
#9246=DIRECTION('ref_axis',(1.,0.,0.));
#9247=DIRECTION('',(0.,0.,-1.));
#9248=DIRECTION('center_axis',(0.,0.,1.));
#9249=DIRECTION('ref_axis',(1.,0.,0.));
#9250=DIRECTION('',(0.,0.,1.));
#9251=DIRECTION('center_axis',(0.,0.,-1.));
#9252=DIRECTION('ref_axis',(0.815134019438135,0.579272414632899,0.));
#9253=DIRECTION('',(0.,0.,-1.));
#9254=DIRECTION('center_axis',(0.,0.,1.));
#9255=DIRECTION('ref_axis',(1.,0.,0.));
#9256=DIRECTION('',(0.,0.,1.));
#9257=DIRECTION('center_axis',(0.,0.,-1.));
#9258=DIRECTION('ref_axis',(-1.,0.,0.));
#9259=DIRECTION('center_axis',(0.,0.,1.));
#9260=DIRECTION('ref_axis',(1.,0.,0.));
#9261=DIRECTION('',(0.,0.,-1.));
#9262=DIRECTION('center_axis',(0.,0.,1.));
#9263=DIRECTION('ref_axis',(1.,0.,0.));
#9264=DIRECTION('',(0.,0.,1.));
#9265=DIRECTION('center_axis',(0.,0.,-1.));
#9266=DIRECTION('ref_axis',(-1.,0.,0.));
#9267=DIRECTION('',(0.,0.,-1.));
#9268=DIRECTION('center_axis',(0.,0.,1.));
#9269=DIRECTION('ref_axis',(1.,0.,0.));
#9270=DIRECTION('',(0.,0.,1.));
#9271=DIRECTION('center_axis',(0.,0.,-1.));
#9272=DIRECTION('ref_axis',(0.815134019438126,-0.579272414632913,0.));
#9273=DIRECTION('center_axis',(0.,0.,1.));
#9274=DIRECTION('ref_axis',(1.,0.,0.));
#9275=DIRECTION('',(0.,0.,-1.));
#9276=DIRECTION('center_axis',(0.,0.,1.));
#9277=DIRECTION('ref_axis',(1.,0.,0.));
#9278=DIRECTION('',(0.,0.,1.));
#9279=DIRECTION('center_axis',(0.,0.,-1.));
#9280=DIRECTION('ref_axis',(-1.,0.,0.));
#9281=DIRECTION('',(0.,0.,-1.));
#9282=DIRECTION('center_axis',(0.,0.,1.));
#9283=DIRECTION('ref_axis',(1.,0.,0.));
#9284=DIRECTION('',(0.,0.,1.));
#9285=DIRECTION('center_axis',(0.,0.,-1.));
#9286=DIRECTION('ref_axis',(0.91775889256032,-0.397138030320008,0.));
#9287=DIRECTION('center_axis',(0.,0.,1.));
#9288=DIRECTION('ref_axis',(-0.998372875767673,0.0570228106233547,0.));
#9289=DIRECTION('',(0.,0.,-1.));
#9290=DIRECTION('center_axis',(0.,0.,1.));
#9291=DIRECTION('ref_axis',(1.,0.,0.));
#9292=DIRECTION('',(0.,0.,1.));
#9293=DIRECTION('center_axis',(0.,0.,-1.));
#9294=DIRECTION('ref_axis',(-1.,0.,0.));
#9295=DIRECTION('',(0.,0.,-1.));
#9296=DIRECTION('center_axis',(0.,0.,1.));
#9297=DIRECTION('ref_axis',(1.,0.,0.));
#9298=DIRECTION('',(0.,0.,1.));
#9299=DIRECTION('center_axis',(0.,0.,-1.));
#9300=DIRECTION('ref_axis',(0.909231636502715,0.416290561005885,0.));
#9301=DIRECTION('center_axis',(0.,0.,1.));
#9302=DIRECTION('ref_axis',(1.,0.,0.));
#9303=DIRECTION('',(0.,0.,-1.));
#9304=DIRECTION('center_axis',(0.,0.,1.));
#9305=DIRECTION('ref_axis',(1.,0.,0.));
#9306=DIRECTION('',(0.,0.,1.));
#9307=DIRECTION('center_axis',(0.,0.,-1.));
#9308=DIRECTION('ref_axis',(-1.,0.,0.));
#9309=DIRECTION('',(0.,0.,-1.));
#9310=DIRECTION('center_axis',(0.,0.,1.));
#9311=DIRECTION('ref_axis',(1.,0.,0.));
#9312=DIRECTION('',(0.,0.,1.));
#9313=DIRECTION('center_axis',(0.,0.,-1.));
#9314=DIRECTION('ref_axis',(0.975914418166611,0.218153726565752,0.));
#9315=DIRECTION('center_axis',(0.,0.,1.));
#9316=DIRECTION('ref_axis',(1.,0.,0.));
#9317=DIRECTION('',(0.,0.,-1.));
#9318=DIRECTION('center_axis',(0.,0.,1.));
#9319=DIRECTION('ref_axis',(1.,0.,0.));
#9320=DIRECTION('',(0.,0.,1.));
#9321=DIRECTION('center_axis',(0.,0.,-1.));
#9322=DIRECTION('ref_axis',(-1.,0.,0.));
#9323=DIRECTION('',(0.,0.,-1.));
#9324=DIRECTION('center_axis',(0.,0.,1.));
#9325=DIRECTION('ref_axis',(1.,0.,0.));
#9326=DIRECTION('',(0.,0.,1.));
#9327=DIRECTION('center_axis',(0.,0.,-1.));
#9328=DIRECTION('ref_axis',(0.98027329818186,-0.197646808402409,0.));
#9329=DIRECTION('center_axis',(0.,0.,1.));
#9330=DIRECTION('ref_axis',(1.,0.,0.));
#9331=DIRECTION('',(0.,0.,-1.));
#9332=DIRECTION('center_axis',(0.,0.,1.));
#9333=DIRECTION('ref_axis',(1.,0.,0.));
#9334=DIRECTION('',(0.,0.,1.));
#9335=DIRECTION('center_axis',(0.,0.,-1.));
#9336=DIRECTION('ref_axis',(-1.,0.,0.));
#9337=DIRECTION('',(0.,0.,-1.));
#9338=DIRECTION('center_axis',(0.,0.,1.));
#9339=DIRECTION('ref_axis',(1.,0.,0.));
#9340=DIRECTION('',(0.,0.,1.));
#9341=DIRECTION('center_axis',(0.,0.,-1.));
#9342=DIRECTION('ref_axis',(0.999945056799679,0.0104825274569784,0.));
#9343=DIRECTION('center_axis',(-1.,0.,0.));
#9344=DIRECTION('ref_axis',(0.,0.,1.));
#9345=DIRECTION('',(0.,0.,1.));
#9346=DIRECTION('center_axis',(0.,1.,0.));
#9347=DIRECTION('ref_axis',(0.,0.,1.));
#9348=DIRECTION('',(0.,0.,1.));
#9349=DIRECTION('center_axis',(1.,0.,0.));
#9350=DIRECTION('ref_axis',(0.,0.,-1.));
#9351=DIRECTION('axis',(0.,0.,1.));
#9352=DIRECTION('refdir',(1.,0.,0.));
#9353=DIRECTION('center_axis',(0.,0.,-1.));
#9354=DIRECTION('ref_axis',(-1.,0.,0.));
#9355=DIRECTION('center_axis',(0.,0.,1.));
#9356=DIRECTION('ref_axis',(1.,0.,0.));
#9357=DIRECTION('',(0.,0.,-1.));
#9358=DIRECTION('center_axis',(0.,0.,1.));
#9359=DIRECTION('ref_axis',(1.,0.,0.));
#9360=DIRECTION('center_axis',(0.,0.,-1.));
#9361=DIRECTION('ref_axis',(-1.,0.,0.));
#9362=DIRECTION('center_axis',(0.,0.,1.));
#9363=DIRECTION('ref_axis',(1.,0.,0.));
#9364=DIRECTION('',(0.,0.,-1.));
#9365=DIRECTION('center_axis',(0.,0.,1.));
#9366=DIRECTION('ref_axis',(1.,0.,0.));
#9367=DIRECTION('',(0.,0.,-1.));
#9368=DIRECTION('center_axis',(0.,0.,1.));
#9369=DIRECTION('ref_axis',(1.,0.,0.));
#9370=DIRECTION('',(0.,0.,1.));
#9371=DIRECTION('center_axis',(0.,0.,1.));
#9372=DIRECTION('ref_axis',(1.,0.,0.));
#9373=DIRECTION('',(0.,0.,-1.));
#9374=DIRECTION('center_axis',(0.,0.,-1.));
#9375=DIRECTION('ref_axis',(-1.,0.,0.));
#9376=DIRECTION('center_axis',(0.,0.,1.));
#9377=DIRECTION('ref_axis',(1.,0.,0.));
#9378=DIRECTION('',(0.,0.,-1.));
#9379=DIRECTION('center_axis',(0.,0.,1.));
#9380=DIRECTION('ref_axis',(1.,0.,0.));
#9381=DIRECTION('center_axis',(0.,0.,1.));
#9382=DIRECTION('ref_axis',(1.,0.,0.));
#9383=DIRECTION('',(0.374606593415916,-0.927183854566786,0.));
#9384=DIRECTION('',(0.927183854566785,0.374606593415917,0.));
#9385=DIRECTION('',(-0.374606593415917,0.927183854566785,0.));
#9386=DIRECTION('',(-0.927183854566787,-0.374606593415913,0.));
#9387=DIRECTION('',(-1.,0.,0.));
#9388=DIRECTION('',(1.,0.,0.));
#9389=DIRECTION('center_axis',(0.,0.,1.));
#9390=DIRECTION('ref_axis',(1.,0.,0.));
#9391=DIRECTION('center_axis',(0.,0.,-1.));
#9392=DIRECTION('ref_axis',(1.,0.,0.));
#9393=DIRECTION('',(0.927183854566786,0.374606593415915,0.));
#9394=DIRECTION('',(0.920504853452439,-0.390731128489277,0.));
#9395=DIRECTION('center_axis',(0.,0.,1.));
#9396=DIRECTION('ref_axis',(1.,0.,0.));
#9397=DIRECTION('',(-1.,0.,0.));
#9398=DIRECTION('',(0.927183854566787,0.374606593415913,0.));
#9399=DIRECTION('',(0.374606593415916,-0.927183854566786,0.));
#9400=DIRECTION('',(0.927183854566787,0.374606593415913,0.));
#9401=DIRECTION('',(-1.,0.,0.));
#9402=DIRECTION('center_axis',(0.,0.,-1.));
#9403=DIRECTION('ref_axis',(1.,0.,0.));
#9404=DIRECTION('',(0.927183854566785,0.374606593415917,0.));
#9405=DIRECTION('',(0.374606593415916,-0.927183854566786,0.));
#9406=DIRECTION('',(0.920504853452439,-0.390731128489277,0.));
#9407=DIRECTION('',(0.927183854566786,0.374606593415915,0.));
#9408=DIRECTION('center_axis',(0.,0.,1.));
#9409=DIRECTION('ref_axis',(-1.,-5.29090660172926E-15,0.));
#9410=DIRECTION('center_axis',(0.,0.,1.));
#9411=DIRECTION('ref_axis',(1.,0.,0.));
#9412=DIRECTION('',(1.,0.,0.));
#9413=DIRECTION('',(-1.,0.,0.));
#9414=DIRECTION('',(-0.927183854566787,-0.374606593415913,0.));
#9415=DIRECTION('',(-0.374606593415917,0.927183854566785,0.));
#9416=DIRECTION('center_axis',(0.,0.,1.));
#9417=DIRECTION('ref_axis',(1.,0.,0.));
#9418=DIRECTION('',(-0.927183854566787,-0.374606593415913,0.));
#9419=DIRECTION('',(-1.,0.,0.));
#9420=DIRECTION('',(-1.,0.,0.));
#9421=DIRECTION('',(0.927183854566787,0.374606593415913,0.));
#9422=DIRECTION('',(0.374606593415916,-0.927183854566786,0.));
#9423=DIRECTION('center_axis',(0.,-1.,0.));
#9424=DIRECTION('ref_axis',(0.,0.,-1.));
#9425=DIRECTION('',(0.,0.,-1.));
#9426=DIRECTION('center_axis',(0.,1.,0.));
#9427=DIRECTION('ref_axis',(0.,0.,1.));
#9428=DIRECTION('',(0.,0.,1.));
#9429=DIRECTION('center_axis',(0.,1.,0.));
#9430=DIRECTION('ref_axis',(0.,0.,1.));
#9431=DIRECTION('',(0.,0.,-1.));
#9432=DIRECTION('center_axis',(0.,-1.,0.));
#9433=DIRECTION('ref_axis',(0.,0.,-1.));
#9434=DIRECTION('',(0.,0.,-1.));
#9435=DIRECTION('center_axis',(0.,0.,-1.));
#9436=DIRECTION('ref_axis',(-1.,0.,0.));
#9437=DIRECTION('',(0.,0.,1.));
#9438=DIRECTION('center_axis',(0.374606593415915,-0.927183854566786,0.));
#9439=DIRECTION('ref_axis',(0.927183854566786,0.374606593415915,0.));
#9440=DIRECTION('',(0.,0.,-1.));
#9441=DIRECTION('',(0.,0.,-1.));
#9442=DIRECTION('center_axis',(0.390731128489276,0.920504853452439,0.));
#9443=DIRECTION('ref_axis',(-0.920504853452439,0.390731128489276,0.));
#9444=DIRECTION('',(0.,0.,-1.));
#9445=DIRECTION('center_axis',(-0.927183854566787,-0.374606593415913,0.));
#9446=DIRECTION('ref_axis',(0.374606593415913,-0.927183854566787,0.));
#9447=DIRECTION('',(0.,0.,1.));
#9448=DIRECTION('',(0.374606593415916,-0.927183854566786,0.));
#9449=DIRECTION('',(0.,0.,-1.));
#9450=DIRECTION('',(0.374606593415916,-0.927183854566786,0.));
#9451=DIRECTION('',(0.,0.,-1.));
#9452=DIRECTION('center_axis',(0.374606593415915,-0.927183854566786,0.));
#9453=DIRECTION('ref_axis',(0.927183854566786,0.374606593415915,0.));
#9454=DIRECTION('',(0.927183854566786,0.374606593415915,0.));
#9455=DIRECTION('',(0.,0.,-1.));
#9456=DIRECTION('',(0.927183854566786,0.374606593415915,0.));
#9457=DIRECTION('center_axis',(0.927183854566786,0.374606593415916,0.));
#9458=DIRECTION('ref_axis',(-0.374606593415916,0.927183854566786,0.));
#9459=DIRECTION('',(0.,0.,-1.));
#9460=DIRECTION('',(0.,0.,-1.));
#9461=DIRECTION('',(-0.374606593415917,0.927183854566785,0.));
#9462=DIRECTION('',(-0.374606593415917,0.927183854566785,0.));
#9463=DIRECTION('',(0.,0.,1.));
#9464=DIRECTION('',(0.,0.,1.));
#9465=DIRECTION('',(0.,0.,-1.));
#9466=DIRECTION('center_axis',(-0.374606593415913,0.927183854566787,0.));
#9467=DIRECTION('ref_axis',(-0.927183854566787,-0.374606593415913,0.));
#9468=DIRECTION('center_axis',(0.374606593415913,-0.927183854566787,0.));
#9469=DIRECTION('ref_axis',(0.927183854566787,0.374606593415913,0.));
#9470=DIRECTION('center_axis',(-0.374606593415913,0.927183854566787,0.));
#9471=DIRECTION('ref_axis',(-0.927183854566787,-0.374606593415913,0.));
#9472=DIRECTION('center_axis',(-0.374606593415917,0.927183854566785,0.));
#9473=DIRECTION('ref_axis',(-0.927183854566785,-0.374606593415917,0.));
#9474=DIRECTION('',(0.927183854566785,0.374606593415917,0.));
#9475=DIRECTION('center_axis',(0.,0.,1.));
#9476=DIRECTION('ref_axis',(1.,0.,0.));
#9477=DIRECTION('center_axis',(0.374606593415917,-0.927183854566785,0.));
#9478=DIRECTION('ref_axis',(0.927183854566785,0.374606593415917,0.));
#9479=DIRECTION('',(0.927183854566785,0.374606593415917,0.));
#9480=DIRECTION('center_axis',(0.,0.,-1.));
#9481=DIRECTION('ref_axis',(1.,0.,0.));
#9482=DIRECTION('center_axis',(0.,0.,-1.));
#9483=DIRECTION('ref_axis',(-1.,0.,0.));
#9484=DIRECTION('axis',(0.,0.,1.));
#9485=DIRECTION('refdir',(1.,0.,0.));
#9486=DIRECTION('center_axis',(0.,0.,-1.));
#9487=DIRECTION('ref_axis',(-1.,0.,0.));
#9488=DIRECTION('center_axis',(0.,0.,1.));
#9489=DIRECTION('ref_axis',(1.,0.,0.));
#9490=DIRECTION('',(0.,0.,1.));
#9491=DIRECTION('center_axis',(0.,0.,1.));
#9492=DIRECTION('ref_axis',(1.,0.,0.));
#9493=DIRECTION('',(0.,0.,1.));
#9494=DIRECTION('center_axis',(0.,0.,-1.));
#9495=DIRECTION('ref_axis',(1.,0.,0.));
#9496=DIRECTION('',(0.,0.,1.));
#9497=DIRECTION('center_axis',(0.,0.,1.));
#9498=DIRECTION('ref_axis',(1.,0.,0.));
#9499=DIRECTION('',(0.,0.,1.));
#9500=DIRECTION('center_axis',(0.,0.,-1.));
#9501=DIRECTION('ref_axis',(1.,0.,0.));
#9502=DIRECTION('',(0.,0.,1.));
#9503=DIRECTION('center_axis',(0.,0.,1.));
#9504=DIRECTION('ref_axis',(1.,0.,0.));
#9505=DIRECTION('center_axis',(0.,0.,-1.));
#9506=DIRECTION('ref_axis',(-1.,0.,0.));
#9507=DIRECTION('center_axis',(0.,0.,1.));
#9508=DIRECTION('ref_axis',(1.,0.,0.));
#9509=DIRECTION('',(0.,0.,1.));
#9510=DIRECTION('center_axis',(0.,0.,1.));
#9511=DIRECTION('ref_axis',(1.,0.,0.));
#9512=DIRECTION('center_axis',(0.,0.,1.));
#9513=DIRECTION('ref_axis',(1.,0.,0.));
#9514=DIRECTION('',(-1.,2.07374770584121E-16,0.));
#9515=DIRECTION('center_axis',(0.,0.,1.));
#9516=DIRECTION('ref_axis',(1.,0.,0.));
#9517=DIRECTION('',(2.07374770584121E-16,-1.,0.));
#9518=DIRECTION('center_axis',(0.,0.,-1.));
#9519=DIRECTION('ref_axis',(-1.,0.,0.));
#9520=DIRECTION('',(0.,0.,1.));
#9521=DIRECTION('center_axis',(0.,0.,1.));
#9522=DIRECTION('ref_axis',(1.,0.,0.));
#9523=DIRECTION('',(0.,0.,1.));
#9524=DIRECTION('center_axis',(0.,0.,1.));
#9525=DIRECTION('ref_axis',(1.,0.,0.));
#9526=DIRECTION('center_axis',(0.,0.,1.));
#9527=DIRECTION('ref_axis',(1.,0.,0.));
#9528=DIRECTION('center_axis',(0.,0.,1.));
#9529=DIRECTION('ref_axis',(1.,0.,0.));
#9530=DIRECTION('',(0.,-1.,0.));
#9531=DIRECTION('center_axis',(0.,0.,1.));
#9532=DIRECTION('ref_axis',(1.,0.,0.));
#9533=DIRECTION('',(0.,1.,0.));
#9534=DIRECTION('center_axis',(0.,0.,-1.));
#9535=DIRECTION('ref_axis',(-1.,0.,0.));
#9536=DIRECTION('center_axis',(0.,0.,1.));
#9537=DIRECTION('ref_axis',(1.,0.,0.));
#9538=DIRECTION('',(0.,0.,-1.));
#9539=DIRECTION('',(0.,0.,-1.));
#9540=DIRECTION('center_axis',(1.,0.,0.));
#9541=DIRECTION('ref_axis',(0.,0.,-1.));
#9542=DIRECTION('',(0.,-1.,0.));
#9543=DIRECTION('',(0.,0.,-1.));
#9544=DIRECTION('center_axis',(0.,0.,-1.));
#9545=DIRECTION('ref_axis',(-1.,0.,0.));
#9546=DIRECTION('center_axis',(0.,0.,1.));
#9547=DIRECTION('ref_axis',(1.,0.,0.));
#9548=DIRECTION('',(0.,0.,-1.));
#9549=DIRECTION('center_axis',(-1.,0.,0.));
#9550=DIRECTION('ref_axis',(0.,0.,1.));
#9551=DIRECTION('',(0.,1.,0.));
#9552=DIRECTION('center_axis',(0.,0.,1.));
#9553=DIRECTION('ref_axis',(1.,0.,0.));
#9554=DIRECTION('center_axis',(0.,0.,1.));
#9555=DIRECTION('ref_axis',(1.,0.,0.));
#9556=DIRECTION('center_axis',(0.,0.,1.));
#9557=DIRECTION('ref_axis',(1.,0.,0.));
#9558=DIRECTION('',(1.,2.07374770584121E-16,0.));
#9559=DIRECTION('',(2.07374770584121E-16,1.,0.));
#9560=DIRECTION('center_axis',(0.,0.,-1.));
#9561=DIRECTION('ref_axis',(0.707106781186548,-0.707106781186547,0.));
#9562=DIRECTION('center_axis',(0.,0.,1.));
#9563=DIRECTION('ref_axis',(1.,0.,0.));
#9564=DIRECTION('',(0.,0.,1.));
#9565=DIRECTION('',(0.,0.,1.));
#9566=DIRECTION('center_axis',(0.,0.,1.));
#9567=DIRECTION('ref_axis',(1.,0.,0.));
#9568=DIRECTION('',(-1.,2.07374770584121E-16,0.));
#9569=DIRECTION('',(1.,2.07374770584121E-16,0.));
#9570=DIRECTION('',(2.07374770584121E-16,1.,0.));
#9571=DIRECTION('',(2.07374770584121E-16,-1.,0.));
#9572=DIRECTION('center_axis',(1.,-2.07374770584121E-16,0.));
#9573=DIRECTION('ref_axis',(2.07374770584121E-16,1.,0.));
#9574=DIRECTION('center_axis',(-1.,-2.07374770584121E-16,0.));
#9575=DIRECTION('ref_axis',(2.07374770584121E-16,-1.,0.));
#9576=DIRECTION('center_axis',(2.07374770584121E-16,1.,0.));
#9577=DIRECTION('ref_axis',(-1.,2.07374770584121E-16,0.));
#9578=DIRECTION('center_axis',(2.07374770584121E-16,-1.,0.));
#9579=DIRECTION('ref_axis',(1.,2.07374770584121E-16,0.));
#9580=DIRECTION('axis',(0.,0.,1.));
#9581=DIRECTION('refdir',(1.,0.,0.));
#9582=DIRECTION('center_axis',(0.,0.,-1.));
#9583=DIRECTION('ref_axis',(-1.,0.,0.));
#9584=DIRECTION('center_axis',(0.,0.,-1.));
#9585=DIRECTION('ref_axis',(1.,0.,0.));
#9586=DIRECTION('',(0.,0.,-1.));
#9587=DIRECTION('center_axis',(0.,0.,-1.));
#9588=DIRECTION('ref_axis',(1.,0.,0.));
#9589=DIRECTION('',(0.,0.,-1.));
#9590=DIRECTION('center_axis',(0.,0.,1.));
#9591=DIRECTION('ref_axis',(1.,0.,0.));
#9592=DIRECTION('center_axis',(0.,0.,-1.));
#9593=DIRECTION('ref_axis',(1.,0.,0.));
#9594=DIRECTION('',(0.,0.,1.));
#9595=DIRECTION('center_axis',(0.,0.,-1.));
#9596=DIRECTION('ref_axis',(1.,0.,0.));
#9597=DIRECTION('',(0.,0.,1.));
#9598=DIRECTION('center_axis',(0.,0.,-1.));
#9599=DIRECTION('ref_axis',(-1.,0.,0.));
#9600=DIRECTION('center_axis',(0.,0.,1.));
#9601=DIRECTION('ref_axis',(1.,0.,0.));
#9602=DIRECTION('',(0.,0.,-1.));
#9603=DIRECTION('center_axis',(0.,0.,1.));
#9604=DIRECTION('ref_axis',(1.,0.,0.));
#9605=DIRECTION('center_axis',(0.,0.,-1.));
#9606=DIRECTION('ref_axis',(-1.,0.,0.));
#9607=DIRECTION('center_axis',(0.,0.,1.));
#9608=DIRECTION('ref_axis',(1.,0.,0.));
#9609=DIRECTION('',(0.,0.,-1.));
#9610=DIRECTION('center_axis',(0.,0.,1.));
#9611=DIRECTION('ref_axis',(1.,0.,0.));
#9612=DIRECTION('center_axis',(0.,0.,-1.));
#9613=DIRECTION('ref_axis',(-1.,0.,0.));
#9614=DIRECTION('center_axis',(0.,0.,1.));
#9615=DIRECTION('ref_axis',(1.,0.,0.));
#9616=DIRECTION('',(0.,0.,-1.));
#9617=DIRECTION('center_axis',(0.,0.,1.));
#9618=DIRECTION('ref_axis',(1.,0.,0.));
#9619=DIRECTION('',(0.,0.,-1.));
#9620=DIRECTION('center_axis',(0.,0.,1.));
#9621=DIRECTION('ref_axis',(1.,0.,0.));
#9622=DIRECTION('',(-1.,0.,0.));
#9623=DIRECTION('center_axis',(0.,0.,1.));
#9624=DIRECTION('ref_axis',(1.,0.,0.));
#9625=DIRECTION('',(1.,0.,0.));
#9626=DIRECTION('center_axis',(0.,0.,-1.));
#9627=DIRECTION('ref_axis',(1.,0.,0.));
#9628=DIRECTION('',(1.,-3.16619526353726E-17,0.));
#9629=DIRECTION('',(-1.,3.16619526353726E-17,0.));
#9630=DIRECTION('center_axis',(0.,-1.,0.));
#9631=DIRECTION('ref_axis',(0.,0.,-1.));
#9632=DIRECTION('',(-1.,0.,0.));
#9633=DIRECTION('',(0.,0.,-1.));
#9634=DIRECTION('center_axis',(0.,1.,0.));
#9635=DIRECTION('ref_axis',(0.,0.,1.));
#9636=DIRECTION('',(0.,0.,-1.));
#9637=DIRECTION('',(1.,0.,0.));
#9638=DIRECTION('center_axis',(0.,0.,-1.));
#9639=DIRECTION('ref_axis',(1.,1.22464679914735E-16,0.));
#9640=DIRECTION('center_axis',(0.,0.,1.));
#9641=DIRECTION('ref_axis',(1.,0.,0.));
#9642=DIRECTION('center_axis',(0.,0.,1.));
#9643=DIRECTION('ref_axis',(1.,0.,0.));
#9644=DIRECTION('',(-1.,3.16619526353726E-17,0.));
#9645=DIRECTION('center_axis',(0.,0.,-1.));
#9646=DIRECTION('ref_axis',(1.,0.,0.));
#9647=DIRECTION('',(1.,-3.16619526353726E-17,0.));
#9648=DIRECTION('center_axis',(3.16619526353726E-17,1.,0.));
#9649=DIRECTION('ref_axis',(-1.,3.16619526353726E-17,0.));
#9650=DIRECTION('',(-1.,3.16619526353726E-17,0.));
#9651=DIRECTION('',(0.,0.,1.));
#9652=DIRECTION('center_axis',(0.,0.,1.));
#9653=DIRECTION('ref_axis',(-1.,1.22464679914735E-16,0.));
#9654=DIRECTION('center_axis',(0.,0.,-1.));
#9655=DIRECTION('ref_axis',(1.,0.,0.));
#9656=DIRECTION('',(0.,0.,1.));
#9657=DIRECTION('center_axis',(-3.16619526353726E-17,-1.,0.));
#9658=DIRECTION('ref_axis',(1.,-3.16619526353726E-17,0.));
#9659=DIRECTION('',(1.,-3.16619526353726E-17,0.));
#9660=DIRECTION('center_axis',(0.,0.,1.));
#9661=DIRECTION('ref_axis',(1.,0.,0.));
#9662=DIRECTION('center_axis',(0.,0.,-1.));
#9663=DIRECTION('ref_axis',(1.,5.66553889764798E-16,0.));
#9664=DIRECTION('',(0.,0.,-1.));
#9665=DIRECTION('center_axis',(0.,0.,-1.));
#9666=DIRECTION('ref_axis',(1.,0.,0.));
#9667=DIRECTION('',(0.,0.,-1.));
#9668=DIRECTION('center_axis',(3.16619526353726E-17,1.,0.));
#9669=DIRECTION('ref_axis',(-1.,3.16619526353726E-17,0.));
#9670=DIRECTION('',(1.,-3.16619526353726E-17,0.));
#9671=DIRECTION('center_axis',(-3.16619526353726E-17,-1.,0.));
#9672=DIRECTION('ref_axis',(1.,-3.16619526353726E-17,0.));
#9673=DIRECTION('',(-1.,3.16619526353726E-17,0.));
#9674=DIRECTION('center_axis',(0.,0.,-1.));
#9675=DIRECTION('ref_axis',(1.,0.,0.));
#9676=DIRECTION('axis',(0.,0.,1.));
#9677=DIRECTION('refdir',(1.,0.,0.));
#9678=DIRECTION('center_axis',(0.,0.,-1.));
#9679=DIRECTION('ref_axis',(-1.,0.,0.));
#9680=DIRECTION('center_axis',(0.,0.,1.));
#9681=DIRECTION('ref_axis',(1.,0.,0.));
#9682=DIRECTION('',(0.,0.,1.));
#9683=DIRECTION('center_axis',(0.,0.,1.));
#9684=DIRECTION('ref_axis',(1.,0.,0.));
#9685=DIRECTION('',(0.,0.,1.));
#9686=DIRECTION('center_axis',(0.,0.,-1.));
#9687=DIRECTION('ref_axis',(1.,0.,0.));
#9688=DIRECTION('',(0.,0.,1.));
#9689=DIRECTION('center_axis',(0.,0.,1.));
#9690=DIRECTION('ref_axis',(1.,0.,0.));
#9691=DIRECTION('',(0.,0.,1.));
#9692=DIRECTION('center_axis',(0.,0.,-1.));
#9693=DIRECTION('ref_axis',(1.,0.,0.));
#9694=DIRECTION('',(0.,0.,1.));
#9695=DIRECTION('center_axis',(0.,0.,1.));
#9696=DIRECTION('ref_axis',(1.,0.,0.));
#9697=DIRECTION('center_axis',(0.,0.,-1.));
#9698=DIRECTION('ref_axis',(-1.,0.,0.));
#9699=DIRECTION('center_axis',(0.,0.,-1.));
#9700=DIRECTION('ref_axis',(-1.,0.,0.));
#9701=DIRECTION('',(0.,0.,1.));
#9702=DIRECTION('center_axis',(0.,0.,1.));
#9703=DIRECTION('ref_axis',(1.,0.,0.));
#9704=DIRECTION('center_axis',(0.,0.,1.));
#9705=DIRECTION('ref_axis',(1.,0.,0.));
#9706=DIRECTION('',(-1.,2.07374770584121E-16,0.));
#9707=DIRECTION('center_axis',(0.,0.,1.));
#9708=DIRECTION('ref_axis',(1.,0.,0.));
#9709=DIRECTION('',(2.07374770584121E-16,-1.,0.));
#9710=DIRECTION('center_axis',(0.,0.,-1.));
#9711=DIRECTION('ref_axis',(-1.,0.,0.));
#9712=DIRECTION('',(0.,0.,1.));
#9713=DIRECTION('center_axis',(0.,0.,1.));
#9714=DIRECTION('ref_axis',(1.,0.,0.));
#9715=DIRECTION('',(0.,0.,1.));
#9716=DIRECTION('center_axis',(0.,0.,1.));
#9717=DIRECTION('ref_axis',(1.,0.,0.));
#9718=DIRECTION('center_axis',(0.,0.,1.));
#9719=DIRECTION('ref_axis',(1.,0.,0.));
#9720=DIRECTION('center_axis',(0.,0.,1.));
#9721=DIRECTION('ref_axis',(1.,0.,0.));
#9722=DIRECTION('',(1.,2.07374770584121E-16,0.));
#9723=DIRECTION('',(2.07374770584121E-16,1.,0.));
#9724=DIRECTION('center_axis',(0.,0.,-1.));
#9725=DIRECTION('ref_axis',(0.707106781186548,-0.707106781186547,0.));
#9726=DIRECTION('center_axis',(0.,0.,1.));
#9727=DIRECTION('ref_axis',(1.,0.,0.));
#9728=DIRECTION('',(0.,0.,1.));
#9729=DIRECTION('',(0.,0.,1.));
#9730=DIRECTION('center_axis',(0.,0.,1.));
#9731=DIRECTION('ref_axis',(1.,0.,0.));
#9732=DIRECTION('',(-1.,2.07374770584121E-16,0.));
#9733=DIRECTION('',(1.,2.07374770584121E-16,0.));
#9734=DIRECTION('',(2.07374770584121E-16,1.,0.));
#9735=DIRECTION('',(2.07374770584121E-16,-1.,0.));
#9736=DIRECTION('center_axis',(1.,-2.07374770584121E-16,0.));
#9737=DIRECTION('ref_axis',(2.07374770584121E-16,1.,0.));
#9738=DIRECTION('center_axis',(-1.,-2.07374770584121E-16,0.));
#9739=DIRECTION('ref_axis',(2.07374770584121E-16,-1.,0.));
#9740=DIRECTION('center_axis',(2.07374770584121E-16,1.,0.));
#9741=DIRECTION('ref_axis',(-1.,2.07374770584121E-16,0.));
#9742=DIRECTION('center_axis',(2.07374770584121E-16,-1.,0.));
#9743=DIRECTION('ref_axis',(1.,2.07374770584121E-16,0.));
#9744=DIRECTION('center_axis',(0.,0.,-1.));
#9745=DIRECTION('ref_axis',(-1.,0.,0.));
#9746=DIRECTION('center_axis',(0.,0.,-1.));
#9747=DIRECTION('ref_axis',(-1.,0.,0.));
#9748=DIRECTION('',(0.,1.,0.));
#9749=DIRECTION('center_axis',(0.,0.,-1.));
#9750=DIRECTION('ref_axis',(-1.,0.,0.));
#9751=DIRECTION('',(0.,-1.,0.));
#9752=DIRECTION('center_axis',(0.,0.,1.));
#9753=DIRECTION('ref_axis',(1.,0.,0.));
#9754=DIRECTION('',(0.,0.,1.));
#9755=DIRECTION('center_axis',(0.,0.,-1.));
#9756=DIRECTION('ref_axis',(-1.,0.,0.));
#9757=DIRECTION('',(0.,0.,1.));
#9758=DIRECTION('center_axis',(-1.,0.,0.));
#9759=DIRECTION('ref_axis',(0.,0.,1.));
#9760=DIRECTION('',(0.,0.,1.));
#9761=DIRECTION('',(0.,-1.,0.));
#9762=DIRECTION('center_axis',(0.,0.,1.));
#9763=DIRECTION('ref_axis',(1.,0.,0.));
#9764=DIRECTION('',(0.,0.,1.));
#9765=DIRECTION('center_axis',(0.,0.,-1.));
#9766=DIRECTION('ref_axis',(-1.,0.,0.));
#9767=DIRECTION('center_axis',(1.,0.,0.));
#9768=DIRECTION('ref_axis',(0.,0.,-1.));
#9769=DIRECTION('',(0.,1.,0.));
#9770=DIRECTION('center_axis',(0.,0.,-1.));
#9771=DIRECTION('ref_axis',(-1.,0.,0.));
#9772=DIRECTION('axis',(0.,0.,1.));
#9773=DIRECTION('refdir',(1.,0.,0.));
#9774=DIRECTION('center_axis',(0.,0.,1.));
#9775=DIRECTION('ref_axis',(1.,0.,0.));
#9776=DIRECTION('center_axis',(0.,0.,1.));
#9777=DIRECTION('ref_axis',(1.,0.,0.));
#9778=DIRECTION('center_axis',(0.,0.,1.));
#9779=DIRECTION('ref_axis',(1.,0.,0.));
#9780=DIRECTION('center_axis',(1.22464679914735E-16,-1.,0.));
#9781=DIRECTION('ref_axis',(-1.,-1.22464679914735E-16,0.));
#9782=DIRECTION('center_axis',(0.,0.,-1.));
#9783=DIRECTION('ref_axis',(1.,0.,0.));
#9784=DIRECTION('center_axis',(0.,0.,-1.));
#9785=DIRECTION('ref_axis',(-1.,0.,0.));
#9786=DIRECTION('center_axis',(0.,0.,1.));
#9787=DIRECTION('ref_axis',(1.,0.,0.));
#9788=DIRECTION('',(0.,0.,-1.));
#9789=DIRECTION('center_axis',(0.,0.,1.));
#9790=DIRECTION('ref_axis',(1.,0.,0.));
#9791=DIRECTION('',(0.,0.,-1.));
#9792=DIRECTION('center_axis',(0.,0.,-1.));
#9793=DIRECTION('ref_axis',(-1.,0.,0.));
#9794=DIRECTION('',(0.,0.,1.));
#9795=DIRECTION('center_axis',(0.,0.,1.));
#9796=DIRECTION('ref_axis',(1.,0.,0.));
#9797=DIRECTION('center_axis',(0.,0.,-1.));
#9798=DIRECTION('ref_axis',(-1.,0.,0.));
#9799=DIRECTION('center_axis',(0.,0.,1.));
#9800=DIRECTION('ref_axis',(1.,0.,0.));
#9801=DIRECTION('',(0.,0.,-1.));
#9802=DIRECTION('center_axis',(0.,0.,1.));
#9803=DIRECTION('ref_axis',(1.,0.,0.));
#9804=DIRECTION('',(0.,0.,-1.));
#9805=DIRECTION('center_axis',(0.,0.,-1.));
#9806=DIRECTION('ref_axis',(-1.,0.,0.));
#9807=DIRECTION('center_axis',(0.,0.,1.));
#9808=DIRECTION('ref_axis',(1.,0.,0.));
#9809=DIRECTION('',(0.,0.,-1.));
#9810=DIRECTION('center_axis',(0.,0.,1.));
#9811=DIRECTION('ref_axis',(1.,0.,0.));
#9812=DIRECTION('',(0.,0.,-1.));
#9813=DIRECTION('center_axis',(0.,0.,1.));
#9814=DIRECTION('ref_axis',(1.,0.,0.));
#9815=DIRECTION('',(0.,0.,-1.));
#9816=DIRECTION('center_axis',(0.,0.,1.));
#9817=DIRECTION('ref_axis',(1.,0.,0.));
#9818=DIRECTION('',(-2.07374770584121E-16,-1.,0.));
#9819=DIRECTION('center_axis',(0.,0.,1.));
#9820=DIRECTION('ref_axis',(1.,0.,0.));
#9821=DIRECTION('',(-2.07374770584121E-16,1.,0.));
#9822=DIRECTION('center_axis',(0.,0.,1.));
#9823=DIRECTION('ref_axis',(1.,0.,0.));
#9824=DIRECTION('',(1.,0.,0.));
#9825=DIRECTION('',(-1.,0.,0.));
#9826=DIRECTION('center_axis',(0.,0.,1.));
#9827=DIRECTION('ref_axis',(1.,0.,0.));
#9828=DIRECTION('',(-2.07374770584121E-16,1.,0.));
#9829=DIRECTION('center_axis',(0.,0.,1.));
#9830=DIRECTION('ref_axis',(1.,0.,0.));
#9831=DIRECTION('',(-2.07374770584121E-16,-1.,0.));
#9832=DIRECTION('',(-1.,0.,0.));
#9833=DIRECTION('',(1.,0.,0.));
#9834=DIRECTION('center_axis',(0.,0.,-1.));
#9835=DIRECTION('ref_axis',(-1.,0.,0.));
#9836=DIRECTION('',(0.,0.,-1.));
#9837=DIRECTION('',(0.,0.,-1.));
#9838=DIRECTION('center_axis',(-1.,-2.07374770584121E-16,0.));
#9839=DIRECTION('ref_axis',(2.07374770584121E-16,-1.,0.));
#9840=DIRECTION('center_axis',(0.,1.,0.));
#9841=DIRECTION('ref_axis',(0.,0.,1.));
#9842=DIRECTION('center_axis',(0.,-1.,0.));
#9843=DIRECTION('ref_axis',(0.,0.,-1.));
#9844=DIRECTION('center_axis',(1.,-2.07374770584121E-16,0.));
#9845=DIRECTION('ref_axis',(2.07374770584121E-16,1.,0.));
#9846=DIRECTION('center_axis',(0.,0.,1.));
#9847=DIRECTION('ref_axis',(1.,0.,0.));
#9848=DIRECTION('center_axis',(0.,0.,-1.));
#9849=DIRECTION('ref_axis',(-1.,0.,0.));
#9850=DIRECTION('',(0.,0.,1.));
#9851=DIRECTION('',(1.,0.,0.));
#9852=DIRECTION('',(0.,0.,1.));
#9853=DIRECTION('',(0.478899407921688,-0.877869783676518,0.));
#9854=DIRECTION('',(6.92149533108846E-18,5.1897381178387E-19,1.));
#9855=DIRECTION('',(-0.28333748371009,0.95902026585721,1.46341266767185E-18));
#9856=DIRECTION('',(1.04997071744882E-22,-7.64649298920801E-22,1.));
#9857=DIRECTION('',(0.382376009742424,0.924006811215946,6.66392799065871E-22));
#9858=DIRECTION('',(-2.57083863150465E-18,-5.63613694710308E-17,1.));
#9859=DIRECTION('',(-0.924006811215946,0.382376009742424,1.91757631559039E-17));
#9860=DIRECTION('',(1.89847568137224E-15,-7.85301121151351E-16,1.));
#9861=DIRECTION('',(0.382376009742427,0.924006811215945,-3.0797083678554E-19));
#9862=DIRECTION('',(0.,0.,-1.));
#9863=DIRECTION('',(-0.993048117845303,-0.117709114531972,0.));
#9864=DIRECTION('',(-1.85630522180545E-21,1.86188991962173E-21,-1.));
#9865=DIRECTION('',(-0.374697031098015,0.927147310240575,2.42179828636357E-21));
#9866=DIRECTION('',(0.,0.,1.));
#9867=DIRECTION('',(1.,0.,0.));
#9868=DIRECTION('',(0.,0.,1.));
#9869=DIRECTION('',(-0.760244359552721,0.649637217043692,0.));
#9870=DIRECTION('',(1.4237867411173E-17,1.8694694221114E-17,1.));
#9871=DIRECTION('',(-0.95902026585721,-0.28333748371009,1.89513110092429E-17));
#9872=DIRECTION('',(0.,0.,1.));
#9873=DIRECTION('',(0.283337483710108,-0.959020265857205,0.));
#9874=DIRECTION('',(0.,0.,-1.));
#9875=DIRECTION('',(0.123009780116061,-0.992405458467354,0.));
#9876=DIRECTION('',(1.0984378404468E-21,-1.09855442061413E-21,1.));
#9877=DIRECTION('',(0.374645775479504,0.927168023022451,6.07019433793157E-22));
#9878=DIRECTION('',(0.,0.,1.));
#9879=DIRECTION('',(0.893341550633277,0.449378319361462,0.));
#9880=DIRECTION('',(0.,0.,1.));
#9881=DIRECTION('',(-0.359526911355771,-0.933134716968016,0.));
#9882=DIRECTION('',(0.,0.,-1.));
#9883=DIRECTION('',(-0.839948312503015,0.542666409798265,0.));
#9884=DIRECTION('',(0.,0.,-1.));
#9885=DIRECTION('',(0.123009780116061,-0.992405458467354,0.));
#9886=DIRECTION('',(0.,0.,1.));
#9887=DIRECTION('',(-0.283588868853752,0.958945959615165,0.));
#9888=DIRECTION('',(2.23983775286451E-19,3.31658470800558E-19,1.));
#9889=DIRECTION('',(0.283588868853753,-0.958945959615165,2.54523245071261E-19));
#9890=DIRECTION('',(1.43248352509334E-22,7.62927833782932E-23,1.));
#9891=DIRECTION('',(0.382591019930888,0.92391780558026,-1.25293794290448E-22));
#9892=DIRECTION('',(0.,0.,1.));
#9893=DIRECTION('',(0.382591019930886,0.923917805580261,0.));
#9894=DIRECTION('',(0.,0.,1.));
#9895=DIRECTION('',(1.,0.,0.));
#9896=DIRECTION('',(0.,0.,1.));
#9897=DIRECTION('',(1.,0.,0.));
#9898=DIRECTION('',(0.,0.,1.));
#9899=DIRECTION('',(1.,0.,0.));
#9900=DIRECTION('',(0.,0.,-1.));
#9901=DIRECTION('',(-0.835562645106847,-0.549395182088493,0.));
#9902=DIRECTION('',(0.,0.,-1.));
#9903=DIRECTION('',(-0.835562645106847,-0.549395182088493,0.));
#9904=DIRECTION('',(0.,0.,-1.));
#9905=DIRECTION('',(-0.835562645106847,-0.549395182088493,0.));
#9906=DIRECTION('',(0.,0.,-1.));
#9907=DIRECTION('',(-0.835562645106847,-0.549395182088493,0.));
#9908=CARTESIAN_POINT('',(0.,0.,0.));
#9909=CARTESIAN_POINT('',(0.,0.,0.));
#9910=CARTESIAN_POINT('Origin',(13.5,-1.65327317884893E-15,5.));
#9911=CARTESIAN_POINT('',(15.,-1.83697019872103E-15,5.));
#9912=CARTESIAN_POINT('Origin',(13.5,-1.65327317884893E-15,5.));
#9913=CARTESIAN_POINT('',(15.,-1.83697019872103E-15,0.));
#9914=CARTESIAN_POINT('',(15.,-1.83697019872103E-15,5.));
#9915=CARTESIAN_POINT('Origin',(13.5,-1.65327317884893E-15,0.));
#9916=CARTESIAN_POINT('Origin',(-5.24999999999999,20.4,5.));
#9917=CARTESIAN_POINT('',(-3.74999999999999,20.4,5.));
#9918=CARTESIAN_POINT('Origin',(-5.24999999999999,20.4,5.));
#9919=CARTESIAN_POINT('',(-3.74999999999999,20.4,0.));
#9920=CARTESIAN_POINT('',(-3.74999999999999,20.4,5.));
#9921=CARTESIAN_POINT('Origin',(-5.24999999999999,20.4,0.));
#9922=CARTESIAN_POINT('Origin',(5.25000000000001,20.4,5.));
#9923=CARTESIAN_POINT('',(6.75000000000001,20.4,5.));
#9924=CARTESIAN_POINT('Origin',(5.25000000000001,20.4,5.));
#9925=CARTESIAN_POINT('',(6.75000000000001,20.4,0.));
#9926=CARTESIAN_POINT('',(6.75000000000001,20.4,5.));
#9927=CARTESIAN_POINT('Origin',(5.25000000000001,20.4,0.));
#9928=CARTESIAN_POINT('Origin',(-13.5,-1.65327317884893E-15,5.));
#9929=CARTESIAN_POINT('',(-12.,-1.83697019872103E-15,5.));
#9930=CARTESIAN_POINT('Origin',(-13.5,-1.65327317884893E-15,5.));
#9931=CARTESIAN_POINT('',(-12.,-1.83697019872103E-15,0.));
#9932=CARTESIAN_POINT('',(-12.,-1.83697019872103E-15,5.));
#9933=CARTESIAN_POINT('Origin',(-13.5,-1.65327317884893E-15,0.));
#9934=CARTESIAN_POINT('Origin',(-25.05,-25.05,5.));
#9935=CARTESIAN_POINT('',(-20.5,-29.6,0.));
#9936=CARTESIAN_POINT('',(-12.5,-37.6,0.));
#9937=CARTESIAN_POINT('',(-25.05,-25.05,0.));
#9938=CARTESIAN_POINT('',(-12.5,-37.6,5.));
#9939=CARTESIAN_POINT('',(-12.5,-37.6,5.));
#9940=CARTESIAN_POINT('',(-20.5,-29.6,5.));
#9941=CARTESIAN_POINT('',(-25.05,-25.05,5.));
#9942=CARTESIAN_POINT('',(-20.5,-29.6,5.));
#9943=CARTESIAN_POINT('Origin',(0.,-37.6,5.));
#9944=CARTESIAN_POINT('',(12.5,-37.6,0.));
#9945=CARTESIAN_POINT('',(0.,-37.6,0.));
#9946=CARTESIAN_POINT('',(12.5,-37.6,5.));
#9947=CARTESIAN_POINT('',(12.5,-37.6,5.));
#9948=CARTESIAN_POINT('',(0.,-37.6,5.));
#9949=CARTESIAN_POINT('Origin',(25.05,-25.05,5.));
#9950=CARTESIAN_POINT('',(20.5,-29.6,0.));
#9951=CARTESIAN_POINT('',(25.05,-25.05,0.));
#9952=CARTESIAN_POINT('',(20.5,-29.6,5.));
#9953=CARTESIAN_POINT('',(20.5,-29.6,5.));
#9954=CARTESIAN_POINT('',(25.05,-25.05,5.));
#9955=CARTESIAN_POINT('Origin',(20.5,-5.26841944555919E-15,5.));
#9956=CARTESIAN_POINT('',(20.5,12.4,0.));
#9957=CARTESIAN_POINT('',(20.5,-5.26841944555919E-15,0.));
#9958=CARTESIAN_POINT('',(20.5,12.4,5.));
#9959=CARTESIAN_POINT('',(20.5,12.4,5.));
#9960=CARTESIAN_POINT('',(20.5,-5.26841944555919E-15,5.));
#9961=CARTESIAN_POINT('Origin',(0.,24.4,5.));
#9962=CARTESIAN_POINT('',(8.5,24.4,5.));
#9963=CARTESIAN_POINT('',(-8.5,24.4,5.));
#9964=CARTESIAN_POINT('',(0.,24.4,5.));
#9965=CARTESIAN_POINT('',(8.5,24.4,0.));
#9966=CARTESIAN_POINT('',(8.5,24.4,5.));
#9967=CARTESIAN_POINT('',(-8.5,24.4,0.));
#9968=CARTESIAN_POINT('',(0.,24.4,0.));
#9969=CARTESIAN_POINT('',(-8.5,24.4,5.));
#9970=CARTESIAN_POINT('Origin',(0.,0.,5.));
#9971=CARTESIAN_POINT('',(13.0833333333333,4.98260864295891,0.));
#9972=CARTESIAN_POINT('',(-13.0833333333333,4.98260864295891,0.));
#9973=CARTESIAN_POINT('Origin',(0.,0.,0.));
#9974=CARTESIAN_POINT('',(13.0833333333333,4.98260864295891,5.));
#9975=CARTESIAN_POINT('',(13.0833333333333,4.98260864295891,5.));
#9976=CARTESIAN_POINT('',(-13.0833333333333,4.98260864295891,5.));
#9977=CARTESIAN_POINT('Origin',(0.,0.,5.));
#9978=CARTESIAN_POINT('',(-13.0833333333333,4.98260864295891,5.));
#9979=CARTESIAN_POINT('Origin',(13.5,-1.65327317884893E-15,5.));
#9980=CARTESIAN_POINT('',(8.73030399291527,1.5,0.));
#9981=CARTESIAN_POINT('Origin',(13.5,-1.65327317884893E-15,0.));
#9982=CARTESIAN_POINT('',(8.73030399291527,1.5,5.));
#9983=CARTESIAN_POINT('',(8.73030399291527,1.5,5.));
#9984=CARTESIAN_POINT('Origin',(13.5,-1.65327317884893E-15,5.));
#9985=CARTESIAN_POINT('Origin',(0.,1.5,5.));
#9986=CARTESIAN_POINT('',(-8.73030399291527,1.5,0.));
#9987=CARTESIAN_POINT('',(0.,1.5,0.));
#9988=CARTESIAN_POINT('',(-8.73030399291527,1.5,5.));
#9989=CARTESIAN_POINT('',(-8.73030399291527,1.5,5.));
#9990=CARTESIAN_POINT('',(0.,1.5,5.));
#9991=CARTESIAN_POINT('Origin',(13.5,-1.65327317884893E-15,5.));
#9992=CARTESIAN_POINT('',(13.0833333333333,-4.98260864295893,0.));
#9993=CARTESIAN_POINT('',(8.73030399291527,-1.5,0.));
#9994=CARTESIAN_POINT('Origin',(13.5,-1.65327317884893E-15,0.));
#9995=CARTESIAN_POINT('',(13.0833333333333,-4.98260864295893,5.));
#9996=CARTESIAN_POINT('',(13.0833333333333,-4.98260864295893,5.));
#9997=CARTESIAN_POINT('',(8.73030399291527,-1.5,5.));
#9998=CARTESIAN_POINT('Origin',(13.5,-1.65327317884893E-15,5.));
#9999=CARTESIAN_POINT('',(8.73030399291527,-1.5,5.));
#10000=CARTESIAN_POINT('Origin',(0.,0.,5.));
#10001=CARTESIAN_POINT('',(-13.0833333333333,-4.98260864295891,0.));
#10002=CARTESIAN_POINT('Origin',(0.,0.,0.));
#10003=CARTESIAN_POINT('',(-13.0833333333333,-4.98260864295891,5.));
#10004=CARTESIAN_POINT('',(-13.0833333333333,-4.98260864295891,5.));
#10005=CARTESIAN_POINT('Origin',(0.,0.,5.));
#10006=CARTESIAN_POINT('Origin',(-13.5,-1.65327317884893E-15,5.));
#10007=CARTESIAN_POINT('',(-8.73030399291527,-1.5,0.));
#10008=CARTESIAN_POINT('Origin',(-13.5,-1.65327317884893E-15,0.));
#10009=CARTESIAN_POINT('',(-8.73030399291527,-1.5,5.));
#10010=CARTESIAN_POINT('',(-8.73030399291527,-1.5,5.));
#10011=CARTESIAN_POINT('Origin',(-13.5,-1.65327317884893E-15,5.));
#10012=CARTESIAN_POINT('Origin',(-20.5,-2.6342097227796E-15,5.));
#10013=CARTESIAN_POINT('',(-20.5,12.4,5.));
#10014=CARTESIAN_POINT('',(-20.5,-2.6342097227796E-15,5.));
#10015=CARTESIAN_POINT('',(-20.5,12.4,0.));
#10016=CARTESIAN_POINT('',(-20.5,12.4,5.));
#10017=CARTESIAN_POINT('',(-20.5,-2.6342097227796E-15,0.));
#10018=CARTESIAN_POINT('Origin',(-13.5,-1.65327317884893E-15,5.));
#10019=CARTESIAN_POINT('Origin',(-13.5,-1.65327317884893E-15,0.));
#10020=CARTESIAN_POINT('Origin',(-13.5,-1.65327317884893E-15,5.));
#10021=CARTESIAN_POINT('Origin',(0.,-1.5,5.));
#10022=CARTESIAN_POINT('',(0.,-1.5,0.));
#10023=CARTESIAN_POINT('',(0.,-1.5,5.));
#10024=CARTESIAN_POINT('Origin',(0.,0.,5.));
#10025=CARTESIAN_POINT('Origin',(8.5,12.4,5.));
#10026=CARTESIAN_POINT('Origin',(-8.5,12.4,5.));
#10027=CARTESIAN_POINT('Origin',(0.,0.,0.));
#10028=CARTESIAN_POINT('Origin',(8.5,12.4,0.));
#10029=CARTESIAN_POINT('Origin',(-8.5,12.4,0.));
#10030=CARTESIAN_POINT('Origin',(8.5,12.4,5.));
#10031=CARTESIAN_POINT('Origin',(-8.5,12.4,5.));
#10032=CARTESIAN_POINT('',(0.,0.,0.));
#10033=CARTESIAN_POINT('Origin',(31.,0.,5.));
#10034=CARTESIAN_POINT('',(34.,-3.67394039744206E-16,3.));
#10035=CARTESIAN_POINT('Origin',(31.,0.,3.));
#10036=CARTESIAN_POINT('',(34.,-3.67394039744206E-16,5.));
#10037=CARTESIAN_POINT('',(34.,-3.67394039744206E-16,5.));
#10038=CARTESIAN_POINT('Origin',(31.,0.,5.));
#10039=CARTESIAN_POINT('Origin',(31.,0.,0.5));
#10040=CARTESIAN_POINT('',(29.197224362268,-3.,0.5));
#10041=CARTESIAN_POINT('',(29.197224362268,3.,0.5));
#10042=CARTESIAN_POINT('Origin',(31.,0.,0.5));
#10043=CARTESIAN_POINT('',(29.197224362268,3.,0.));
#10044=CARTESIAN_POINT('',(29.197224362268,3.,0.5));
#10045=CARTESIAN_POINT('',(29.197224362268,-3.,0.));
#10046=CARTESIAN_POINT('Origin',(31.,0.,0.));
#10047=CARTESIAN_POINT('',(29.197224362268,-3.,0.5));
#10048=CARTESIAN_POINT('Origin',(0.,0.,2.5));
#10049=CARTESIAN_POINT('',(1.80277563773199,3.,2.5));
#10050=CARTESIAN_POINT('',(1.802775637732,-3.,2.5));
#10051=CARTESIAN_POINT('Origin',(0.,0.,2.5));
#10052=CARTESIAN_POINT('',(1.80277563773199,3.,3.));
#10053=CARTESIAN_POINT('',(1.80277563773199,3.,2.5));
#10054=CARTESIAN_POINT('',(1.802775637732,-3.,3.));
#10055=CARTESIAN_POINT('Origin',(0.,0.,3.));
#10056=CARTESIAN_POINT('',(1.802775637732,-3.,2.5));
#10057=CARTESIAN_POINT('Origin',(31.,0.,3.));
#10058=CARTESIAN_POINT('',(32.5,-1.83697019872104E-16,5.));
#10059=CARTESIAN_POINT('Origin',(31.,0.,5.));
#10060=CARTESIAN_POINT('',(32.5,-1.83697019872104E-16,0.));
#10061=CARTESIAN_POINT('',(32.5,-1.83697019872104E-16,3.));
#10062=CARTESIAN_POINT('Origin',(31.,0.,0.));
#10063=CARTESIAN_POINT('Origin',(0.,0.,3.));
#10064=CARTESIAN_POINT('',(1.5,-1.83697019872103E-16,5.));
#10065=CARTESIAN_POINT('Origin',(0.,0.,5.));
#10066=CARTESIAN_POINT('',(1.5,-1.83697019872103E-16,0.));
#10067=CARTESIAN_POINT('',(1.5,-1.83697019872103E-16,3.));
#10068=CARTESIAN_POINT('Origin',(0.,0.,0.));
#10069=CARTESIAN_POINT('Origin',(0.,0.,3.));
#10070=CARTESIAN_POINT('',(-3.35410196624968,1.,3.));
#10071=CARTESIAN_POINT('',(-3.35410196624968,-1.,3.));
#10072=CARTESIAN_POINT('Origin',(0.,0.,3.));
#10073=CARTESIAN_POINT('',(0.,3.5,3.));
#10074=CARTESIAN_POINT('Origin',(0.,0.,3.));
#10075=CARTESIAN_POINT('',(0.,3.5,0.));
#10076=CARTESIAN_POINT('',(0.,3.5,3.));
#10077=CARTESIAN_POINT('',(0.,-3.5,0.));
#10078=CARTESIAN_POINT('Origin',(0.,0.,0.));
#10079=CARTESIAN_POINT('',(0.,-3.5,3.));
#10080=CARTESIAN_POINT('',(0.,-3.5,3.));
#10081=CARTESIAN_POINT('Origin',(0.,0.,3.));
#10082=CARTESIAN_POINT('Origin',(0.,0.,3.));
#10083=CARTESIAN_POINT('',(-2.82842712474619,-1.,3.));
#10084=CARTESIAN_POINT('',(-2.82842712474619,1.,3.));
#10085=CARTESIAN_POINT('Origin',(0.,0.,3.));
#10086=CARTESIAN_POINT('',(0.,-1.,3.));
#10087=CARTESIAN_POINT('',(31.,-3.5,3.));
#10088=CARTESIAN_POINT('',(31.,-3.5,3.));
#10089=CARTESIAN_POINT('',(31.,3.5,3.));
#10090=CARTESIAN_POINT('Origin',(31.,0.,3.));
#10091=CARTESIAN_POINT('',(0.,3.5,3.));
#10092=CARTESIAN_POINT('',(0.,1.,3.));
#10093=CARTESIAN_POINT('',(29.197224362268,-3.,3.));
#10094=CARTESIAN_POINT('',(29.197224362268,3.,3.));
#10095=CARTESIAN_POINT('Origin',(31.,0.,3.));
#10096=CARTESIAN_POINT('',(1.802775637732,-3.,3.));
#10097=CARTESIAN_POINT('',(1.802775637732,3.,3.));
#10098=CARTESIAN_POINT('Origin',(0.,0.,0.));
#10099=CARTESIAN_POINT('',(31.,3.5,0.));
#10100=CARTESIAN_POINT('',(0.,3.5,0.));
#10101=CARTESIAN_POINT('',(31.,-3.5,0.));
#10102=CARTESIAN_POINT('Origin',(31.,0.,0.));
#10103=CARTESIAN_POINT('',(31.,-3.5,0.));
#10104=CARTESIAN_POINT('',(1.80277563773199,3.,0.));
#10105=CARTESIAN_POINT('',(1.802775637732,3.,0.));
#10106=CARTESIAN_POINT('',(1.802775637732,-3.,0.));
#10107=CARTESIAN_POINT('Origin',(0.,0.,0.));
#10108=CARTESIAN_POINT('',(1.802775637732,-3.,0.));
#10109=CARTESIAN_POINT('Origin',(31.,-3.5,3.));
#10110=CARTESIAN_POINT('',(31.,-3.5,3.));
#10111=CARTESIAN_POINT('Origin',(31.,0.,3.));
#10112=CARTESIAN_POINT('',(31.,3.5,3.));
#10113=CARTESIAN_POINT('Origin',(0.,3.5,3.));
#10114=CARTESIAN_POINT('Origin',(31.,0.,2.5));
#10115=CARTESIAN_POINT('',(29.197224362268,3.,2.5));
#10116=CARTESIAN_POINT('',(29.197224362268,3.,2.5));
#10117=CARTESIAN_POINT('',(29.197224362268,-3.,2.5));
#10118=CARTESIAN_POINT('Origin',(31.,0.,2.5));
#10119=CARTESIAN_POINT('',(29.197224362268,-3.,2.5));
#10120=CARTESIAN_POINT('Origin',(1.802775637732,-3.,2.5));
#10121=CARTESIAN_POINT('',(1.802775637732,-3.,2.5));
#10122=CARTESIAN_POINT('Origin',(1.802775637732,3.,2.5));
#10123=CARTESIAN_POINT('',(1.802775637732,3.,2.5));
#10124=CARTESIAN_POINT('Origin',(31.,0.,2.5));
#10125=CARTESIAN_POINT('Origin',(1.802775637732,3.,0.5));
#10126=CARTESIAN_POINT('',(1.80277563773199,3.,0.5));
#10127=CARTESIAN_POINT('',(1.802775637732,3.,0.5));
#10128=CARTESIAN_POINT('',(1.80277563773199,3.,0.5));
#10129=CARTESIAN_POINT('Origin',(0.,0.,0.5));
#10130=CARTESIAN_POINT('',(1.802775637732,-3.,0.5));
#10131=CARTESIAN_POINT('Origin',(0.,0.,0.5));
#10132=CARTESIAN_POINT('',(1.802775637732,-3.,0.5));
#10133=CARTESIAN_POINT('Origin',(1.802775637732,-3.,0.5));
#10134=CARTESIAN_POINT('',(1.802775637732,-3.,0.5));
#10135=CARTESIAN_POINT('Origin',(31.,0.,0.5));
#10136=CARTESIAN_POINT('Origin',(0.,0.,3.));
#10137=CARTESIAN_POINT('',(-4.,1.,3.));
#10138=CARTESIAN_POINT('',(0.,1.,3.));
#10139=CARTESIAN_POINT('',(-4.,-1.,3.));
#10140=CARTESIAN_POINT('',(0.,-1.,3.));
#10141=CARTESIAN_POINT('',(-4.,0.,3.));
#10142=CARTESIAN_POINT('Origin',(0.,-1.,5.));
#10143=CARTESIAN_POINT('',(-2.82842712474619,-1.,5.));
#10144=CARTESIAN_POINT('',(-2.82842712474619,-1.,5.));
#10145=CARTESIAN_POINT('',(-4.,-1.,5.));
#10146=CARTESIAN_POINT('',(0.,-1.,5.));
#10147=CARTESIAN_POINT('',(-4.,-1.,5.));
#10148=CARTESIAN_POINT('Origin',(0.,0.,5.));
#10149=CARTESIAN_POINT('',(-2.82842712474619,1.,5.));
#10150=CARTESIAN_POINT('',(-2.82842712474619,1.,5.));
#10151=CARTESIAN_POINT('Origin',(0.,0.,5.));
#10152=CARTESIAN_POINT('Origin',(0.,1.,5.));
#10153=CARTESIAN_POINT('',(-4.,1.,5.));
#10154=CARTESIAN_POINT('',(-4.,1.,5.));
#10155=CARTESIAN_POINT('',(0.,1.,5.));
#10156=CARTESIAN_POINT('Origin',(-4.,0.,5.));
#10157=CARTESIAN_POINT('',(-4.,0.,5.));
#10158=CARTESIAN_POINT('Origin',(0.,0.,5.));
#10159=CARTESIAN_POINT('Origin',(0.,0.,5.));
#10160=CARTESIAN_POINT('',(0.,0.,0.));
#10161=CARTESIAN_POINT('Origin',(-12.5,-8.67361737988404E-16,2.5));
#10162=CARTESIAN_POINT('',(-11.,-1.05105875786051E-15,2.5));
#10163=CARTESIAN_POINT('Origin',(-12.5,-8.67361737988404E-16,2.5));
#10164=CARTESIAN_POINT('',(-11.,-1.05105875786051E-15,0.));
#10165=CARTESIAN_POINT('',(-11.,-1.05105875786051E-15,2.5));
#10166=CARTESIAN_POINT('Origin',(-12.5,-8.67361737988404E-16,0.));
#10167=CARTESIAN_POINT('Origin',(-12.5,-8.67361737988404E-16,2.5));
#10168=CARTESIAN_POINT('',(-12.5,3.5,2.5));
#10169=CARTESIAN_POINT('',(-12.5,-3.5,2.5));
#10170=CARTESIAN_POINT('Origin',(-12.5,-8.67361737988404E-16,2.5));
#10171=CARTESIAN_POINT('',(-12.5,3.5,0.));
#10172=CARTESIAN_POINT('',(-12.5,3.5,2.5));
#10173=CARTESIAN_POINT('',(-12.5,-3.5,0.));
#10174=CARTESIAN_POINT('Origin',(-12.5,-8.67361737988404E-16,0.));
#10175=CARTESIAN_POINT('',(-12.5,-3.5,2.5));
#10176=CARTESIAN_POINT('Origin',(31.,0.,5.));
#10177=CARTESIAN_POINT('',(34.,-3.67394039744206E-16,3.));
#10178=CARTESIAN_POINT('Origin',(31.,0.,3.));
#10179=CARTESIAN_POINT('',(34.,-3.67394039744206E-16,5.));
#10180=CARTESIAN_POINT('',(34.,-3.67394039744206E-16,5.));
#10181=CARTESIAN_POINT('Origin',(31.,0.,5.));
#10182=CARTESIAN_POINT('Origin',(31.,0.,0.5));
#10183=CARTESIAN_POINT('',(29.197224362268,-3.,0.5));
#10184=CARTESIAN_POINT('',(29.197224362268,3.,0.5));
#10185=CARTESIAN_POINT('Origin',(31.,0.,0.5));
#10186=CARTESIAN_POINT('',(29.197224362268,3.,0.));
#10187=CARTESIAN_POINT('',(29.197224362268,3.,0.5));
#10188=CARTESIAN_POINT('',(29.197224362268,-3.,0.));
#10189=CARTESIAN_POINT('Origin',(31.,0.,0.));
#10190=CARTESIAN_POINT('',(29.197224362268,-3.,0.5));
#10191=CARTESIAN_POINT('Origin',(0.,0.,2.5));
#10192=CARTESIAN_POINT('',(1.80277563773199,3.,2.5));
#10193=CARTESIAN_POINT('',(1.802775637732,-3.,2.5));
#10194=CARTESIAN_POINT('Origin',(0.,0.,2.5));
#10195=CARTESIAN_POINT('',(1.80277563773199,3.,3.));
#10196=CARTESIAN_POINT('',(1.80277563773199,3.,2.5));
#10197=CARTESIAN_POINT('',(1.802775637732,-3.,3.));
#10198=CARTESIAN_POINT('Origin',(0.,0.,3.));
#10199=CARTESIAN_POINT('',(1.802775637732,-3.,2.5));
#10200=CARTESIAN_POINT('Origin',(31.,0.,3.));
#10201=CARTESIAN_POINT('',(32.5,-1.83697019872104E-16,5.));
#10202=CARTESIAN_POINT('Origin',(31.,0.,5.));
#10203=CARTESIAN_POINT('',(32.5,-1.83697019872104E-16,0.));
#10204=CARTESIAN_POINT('',(32.5,-1.83697019872104E-16,3.));
#10205=CARTESIAN_POINT('Origin',(31.,0.,0.));
#10206=CARTESIAN_POINT('Origin',(0.,0.,3.));
#10207=CARTESIAN_POINT('',(1.5,-1.83697019872103E-16,5.));
#10208=CARTESIAN_POINT('Origin',(0.,0.,5.));
#10209=CARTESIAN_POINT('',(1.5,-1.83697019872103E-16,0.));
#10210=CARTESIAN_POINT('',(1.5,-1.83697019872103E-16,3.));
#10211=CARTESIAN_POINT('Origin',(0.,0.,0.));
#10212=CARTESIAN_POINT('Origin',(0.,0.,2.5));
#10213=CARTESIAN_POINT('',(-4.,-3.5,2.5));
#10214=CARTESIAN_POINT('',(-12.5,-3.5,2.5));
#10215=CARTESIAN_POINT('',(-4.,3.5,2.5));
#10216=CARTESIAN_POINT('',(-4.,-3.5,2.5));
#10217=CARTESIAN_POINT('',(0.,3.5,2.5));
#10218=CARTESIAN_POINT('Origin',(0.,0.,3.));
#10219=CARTESIAN_POINT('',(-2.82842712474619,-1.,3.));
#10220=CARTESIAN_POINT('',(-2.82842712474619,1.,3.));
#10221=CARTESIAN_POINT('Origin',(0.,0.,3.));
#10222=CARTESIAN_POINT('',(-4.,-1.,3.));
#10223=CARTESIAN_POINT('',(0.,-1.,3.));
#10224=CARTESIAN_POINT('',(-4.,-3.5,3.));
#10225=CARTESIAN_POINT('',(-4.,-3.5,3.));
#10226=CARTESIAN_POINT('',(31.,-3.5,3.));
#10227=CARTESIAN_POINT('',(31.,-3.5,3.));
#10228=CARTESIAN_POINT('',(31.,3.5,3.));
#10229=CARTESIAN_POINT('Origin',(31.,0.,3.));
#10230=CARTESIAN_POINT('',(-4.,3.5,3.));
#10231=CARTESIAN_POINT('',(0.,3.5,3.));
#10232=CARTESIAN_POINT('',(-4.,1.,3.));
#10233=CARTESIAN_POINT('',(-4.,-3.5,3.));
#10234=CARTESIAN_POINT('',(0.,1.,3.));
#10235=CARTESIAN_POINT('',(29.197224362268,-3.,3.));
#10236=CARTESIAN_POINT('',(29.197224362268,3.,3.));
#10237=CARTESIAN_POINT('Origin',(31.,0.,3.));
#10238=CARTESIAN_POINT('',(1.802775637732,-3.,3.));
#10239=CARTESIAN_POINT('',(1.802775637732,3.,3.));
#10240=CARTESIAN_POINT('Origin',(0.,0.,0.));
#10241=CARTESIAN_POINT('',(31.,-3.5,0.));
#10242=CARTESIAN_POINT('',(31.,-3.5,0.));
#10243=CARTESIAN_POINT('',(31.,3.5,0.));
#10244=CARTESIAN_POINT('',(0.,3.5,0.));
#10245=CARTESIAN_POINT('Origin',(31.,0.,0.));
#10246=CARTESIAN_POINT('',(1.80277563773199,3.,0.));
#10247=CARTESIAN_POINT('',(1.802775637732,3.,0.));
#10248=CARTESIAN_POINT('',(1.802775637732,-3.,0.));
#10249=CARTESIAN_POINT('Origin',(0.,0.,0.));
#10250=CARTESIAN_POINT('',(1.802775637732,-3.,0.));
#10251=CARTESIAN_POINT('Origin',(31.,-3.5,3.));
#10252=CARTESIAN_POINT('',(31.,-3.5,3.));
#10253=CARTESIAN_POINT('',(-4.,-3.5,3.));
#10254=CARTESIAN_POINT('Origin',(31.,0.,3.));
#10255=CARTESIAN_POINT('',(31.,3.5,3.));
#10256=CARTESIAN_POINT('Origin',(0.,3.5,3.));
#10257=CARTESIAN_POINT('',(-4.,3.5,3.));
#10258=CARTESIAN_POINT('Origin',(31.,0.,2.5));
#10259=CARTESIAN_POINT('',(29.197224362268,3.,2.5));
#10260=CARTESIAN_POINT('',(29.197224362268,3.,2.5));
#10261=CARTESIAN_POINT('',(29.197224362268,-3.,2.5));
#10262=CARTESIAN_POINT('Origin',(31.,0.,2.5));
#10263=CARTESIAN_POINT('',(29.197224362268,-3.,2.5));
#10264=CARTESIAN_POINT('Origin',(1.802775637732,-3.,2.5));
#10265=CARTESIAN_POINT('',(1.802775637732,-3.,2.5));
#10266=CARTESIAN_POINT('Origin',(1.802775637732,3.,2.5));
#10267=CARTESIAN_POINT('',(1.802775637732,3.,2.5));
#10268=CARTESIAN_POINT('Origin',(31.,0.,2.5));
#10269=CARTESIAN_POINT('Origin',(1.802775637732,3.,0.5));
#10270=CARTESIAN_POINT('',(1.80277563773199,3.,0.5));
#10271=CARTESIAN_POINT('',(1.802775637732,3.,0.5));
#10272=CARTESIAN_POINT('',(1.80277563773199,3.,0.5));
#10273=CARTESIAN_POINT('Origin',(0.,0.,0.5));
#10274=CARTESIAN_POINT('',(1.802775637732,-3.,0.5));
#10275=CARTESIAN_POINT('Origin',(0.,0.,0.5));
#10276=CARTESIAN_POINT('',(1.802775637732,-3.,0.5));
#10277=CARTESIAN_POINT('Origin',(1.802775637732,-3.,0.5));
#10278=CARTESIAN_POINT('',(1.802775637732,-3.,0.5));
#10279=CARTESIAN_POINT('Origin',(31.,0.,0.5));
#10280=CARTESIAN_POINT('Origin',(0.,-1.,5.));
#10281=CARTESIAN_POINT('',(-2.82842712474619,-1.,5.));
#10282=CARTESIAN_POINT('',(-2.82842712474619,-1.,5.));
#10283=CARTESIAN_POINT('',(-4.,-1.,5.));
#10284=CARTESIAN_POINT('',(0.,-1.,5.));
#10285=CARTESIAN_POINT('',(-4.,-1.,5.));
#10286=CARTESIAN_POINT('Origin',(0.,0.,5.));
#10287=CARTESIAN_POINT('',(-2.82842712474619,1.,5.));
#10288=CARTESIAN_POINT('',(-2.82842712474619,1.,5.));
#10289=CARTESIAN_POINT('Origin',(0.,0.,5.));
#10290=CARTESIAN_POINT('Origin',(0.,1.,5.));
#10291=CARTESIAN_POINT('',(-4.,1.,5.));
#10292=CARTESIAN_POINT('',(-4.,1.,5.));
#10293=CARTESIAN_POINT('',(0.,1.,5.));
#10294=CARTESIAN_POINT('Origin',(-4.,0.,5.));
#10295=CARTESIAN_POINT('',(-4.,0.,5.));
#10296=CARTESIAN_POINT('Origin',(0.,0.,5.));
#10297=CARTESIAN_POINT('Origin',(0.,0.,5.));
#10298=CARTESIAN_POINT('',(0.,0.,0.));
#10299=CARTESIAN_POINT('Origin',(1.58293517182884E-14,-0.0809177714881197,
-0.999999999999996));
#10300=CARTESIAN_POINT('',(-0.749999999999984,2.82381973816744,-0.999999999999996));
#10301=CARTESIAN_POINT('',(0.750000000000016,2.82381973816744,-0.999999999999996));
#10302=CARTESIAN_POINT('Origin',(1.56865040007378E-14,-0.0809177714881158,
-0.999999999999996));
#10303=CARTESIAN_POINT('',(-0.749999999999984,2.82381973816744,1.));
#10304=CARTESIAN_POINT('',(-0.749999999999984,2.82381973816744,-0.999999999999996));
#10305=CARTESIAN_POINT('',(0.750000000000016,2.82381973816744,1.));
#10306=CARTESIAN_POINT('Origin',(1.56865040007378E-14,-0.0809177714881158,
1.));
#10307=CARTESIAN_POINT('',(0.750000000000016,2.82381973816744,-0.999999999999996));
#10308=CARTESIAN_POINT('Origin',(2.39698905616068,12.3348169415543,-0.999999999999996));
#10309=CARTESIAN_POINT('',(2.34580779517504,12.0697122857598,1.));
#10310=CARTESIAN_POINT('',(2.12840559486948,12.3624380262694,1.));
#10311=CARTESIAN_POINT('Origin',(2.39698905616068,12.3348169415543,1.));
#10312=CARTESIAN_POINT('',(2.34580779517504,12.0697122857598,-0.999999999999996));
#10313=CARTESIAN_POINT('',(2.34580779517504,12.0697122857598,-0.999999999999996));
#10314=CARTESIAN_POINT('',(2.12840559486948,12.3624380262694,-0.999999999999996));
#10315=CARTESIAN_POINT('Origin',(2.39698905616068,12.3348169415543,-0.999999999999996));
#10316=CARTESIAN_POINT('',(2.12840559486948,12.3624380262694,-0.999999999999996));
#10317=CARTESIAN_POINT('Origin',(-1.53976292115091,12.7396719514087,-0.999999999999996));
#10318=CARTESIAN_POINT('',(1.84616149105017,14.2002477183787,-0.999999999999996));
#10319=CARTESIAN_POINT('Origin',(-1.5397629211509,12.7396719514087,-0.999999999999996));
#10320=CARTESIAN_POINT('',(1.84616149105017,14.2002477183787,1.));
#10321=CARTESIAN_POINT('',(1.84616149105017,14.2002477183787,4.11429224827654E-15));
#10322=CARTESIAN_POINT('Origin',(-1.53976292115089,12.7396719514087,1.));
#10323=CARTESIAN_POINT('Origin',(4.92598549120215,11.5651413018837,-0.999999999999996));
#10324=CARTESIAN_POINT('',(4.82080430633663,11.3164710013847,1.));
#10325=CARTESIAN_POINT('',(4.66901396936873,11.6480004411902,1.));
#10326=CARTESIAN_POINT('Origin',(4.92598549120215,11.5651413018837,1.));
#10327=CARTESIAN_POINT('',(4.82080430633663,11.3164710013847,-0.999999999999996));
#10328=CARTESIAN_POINT('',(4.82080430633663,11.3164710013847,-0.999999999999996));
#10329=CARTESIAN_POINT('',(4.66901396936873,11.6480004411902,-0.999999999999996));
#10330=CARTESIAN_POINT('Origin',(4.92598549120215,11.5651413018837,-0.999999999999996));
#10331=CARTESIAN_POINT('',(4.66901396936873,11.6480004411902,-0.999999999999996));
#10332=CARTESIAN_POINT('Origin',(1.15943507954564,12.7796460183509,-0.999999999999996));
#10333=CARTESIAN_POINT('',(4.77503969688432,13.5043314309807,-0.999999999999996));
#10334=CARTESIAN_POINT('Origin',(1.15943507954563,12.7796460183509,-0.999999999999996));
#10335=CARTESIAN_POINT('',(4.77503969688432,13.5043314309807,1.));
#10336=CARTESIAN_POINT('',(4.77503969688432,13.5043314309807,4.11429224827654E-15));
#10337=CARTESIAN_POINT('Origin',(1.15943507954562,12.7796460183509,1.));
#10338=CARTESIAN_POINT('Origin',(2.39698905616043,-12.4966524845306,-0.999999999999996));
#10339=CARTESIAN_POINT('',(2.12840559486923,-12.5242735692457,1.));
#10340=CARTESIAN_POINT('',(2.34580779517479,-12.2315478287361,1.));
#10341=CARTESIAN_POINT('Origin',(2.39698905616042,-12.4966524845306,1.));
#10342=CARTESIAN_POINT('',(2.12840559486923,-12.5242735692457,-0.999999999999996));
#10343=CARTESIAN_POINT('',(2.12840559486923,-12.5242735692457,-0.999999999999996));
#10344=CARTESIAN_POINT('',(2.34580779517479,-12.2315478287361,-0.999999999999996));
#10345=CARTESIAN_POINT('Origin',(2.39698905616042,-12.4966524845306,-0.999999999999996));
#10346=CARTESIAN_POINT('',(2.34580779517479,-12.2315478287361,-0.999999999999996));
#10347=CARTESIAN_POINT('Origin',(-1.53976292115116,-12.9015074943849,-0.999999999999996));
#10348=CARTESIAN_POINT('',(1.84616149104988,-14.362083261355,-0.999999999999996));
#10349=CARTESIAN_POINT('Origin',(-1.53976292115115,-12.9015074943849,-1.));
#10350=CARTESIAN_POINT('',(1.84616149104989,-14.362083261355,1.));
#10351=CARTESIAN_POINT('Origin',(-1.53976292115116,-12.9015074943849,1.));
#10352=CARTESIAN_POINT('',(1.84616149104988,-14.362083261355,4.11429224827654E-15));
#10353=CARTESIAN_POINT('Origin',(4.92598549120192,-11.72697684486,-0.999999999999996));
#10354=CARTESIAN_POINT('',(4.66901396936849,-11.8098359841665,1.));
#10355=CARTESIAN_POINT('',(4.8208043063364,-11.478306544361,1.));
#10356=CARTESIAN_POINT('Origin',(4.92598549120192,-11.72697684486,1.));
#10357=CARTESIAN_POINT('',(4.66901396936849,-11.8098359841665,-0.999999999999996));
#10358=CARTESIAN_POINT('',(4.66901396936849,-11.8098359841665,-0.999999999999996));
#10359=CARTESIAN_POINT('',(4.8208043063364,-11.478306544361,-0.999999999999996));
#10360=CARTESIAN_POINT('Origin',(4.92598549120192,-11.72697684486,-0.999999999999996));
#10361=CARTESIAN_POINT('',(4.8208043063364,-11.478306544361,-0.999999999999996));
#10362=CARTESIAN_POINT('Origin',(1.15943507954538,-12.9414815613272,-0.999999999999996));
#10363=CARTESIAN_POINT('',(4.77503969688405,-13.666166973957,-0.999999999999996));
#10364=CARTESIAN_POINT('Origin',(1.15943507954539,-12.9414815613271,-0.999999999999996));
#10365=CARTESIAN_POINT('',(4.77503969688405,-13.666166973957,1.));
#10366=CARTESIAN_POINT('Origin',(1.15943507954538,-12.9414815613272,1.00000000000001));
#10367=CARTESIAN_POINT('',(4.77503969688405,-13.666166973957,4.11429224827654E-15));
#10368=CARTESIAN_POINT('Origin',(9.23699064246663,-8.71654333487287,-0.999999999999996));
#10369=CARTESIAN_POINT('',(9.03593732412188,-8.89675865936711,1.));
#10370=CARTESIAN_POINT('',(9.03975952554564,-8.53215275344828,1.));
#10371=CARTESIAN_POINT('Origin',(9.23699064246663,-8.71654333487287,1.));
#10372=CARTESIAN_POINT('',(9.03593732412188,-8.89675865936711,-0.999999999999996));
#10373=CARTESIAN_POINT('',(9.03593732412188,-8.89675865936711,-0.999999999999996));
#10374=CARTESIAN_POINT('',(9.03975952554564,-8.53215275344828,-0.999999999999996));
#10375=CARTESIAN_POINT('Origin',(9.23699064246663,-8.71654333487287,-0.999999999999996));
#10376=CARTESIAN_POINT('',(9.03975952554564,-8.53215275344828,-0.999999999999996));
#10377=CARTESIAN_POINT('Origin',(7.23969272277696,-10.4483125396915,-0.999999999999996));
#10378=CARTESIAN_POINT('',(7.0055640289916,-10.5827883915994,1.));
#10379=CARTESIAN_POINT('',(7.0851085365255,-10.2269446798722,1.));
#10380=CARTESIAN_POINT('Origin',(7.23969272277696,-10.4483125396915,1.));
#10381=CARTESIAN_POINT('',(7.0055640289916,-10.5827883915994,-0.999999999999996));
#10382=CARTESIAN_POINT('',(7.0055640289916,-10.5827883915994,-0.999999999999996));
#10383=CARTESIAN_POINT('',(7.0851085365255,-10.2269446798722,-0.999999999999996));
#10384=CARTESIAN_POINT('Origin',(7.23969272277696,-10.4483125396915,-0.999999999999996));
#10385=CARTESIAN_POINT('',(7.0851085365255,-10.2269446798722,-0.999999999999996));
#10386=CARTESIAN_POINT('Origin',(10.8305877470817,-6.60735585460537,-0.999999999999996));
#10387=CARTESIAN_POINT('',(10.6713967989501,-6.82543437723646,1.));
#10388=CARTESIAN_POINT('',(10.5993296457206,-6.46800130478792,1.));
#10389=CARTESIAN_POINT('Origin',(10.8305877470817,-6.60735585460537,1.));
#10390=CARTESIAN_POINT('',(10.6713967989501,-6.82543437723646,-0.999999999999996));
#10391=CARTESIAN_POINT('',(10.6713967989501,-6.82543437723646,-0.999999999999996));
#10392=CARTESIAN_POINT('',(10.5993296457206,-6.46800130478792,-0.999999999999996));
#10393=CARTESIAN_POINT('Origin',(10.8305877470817,-6.60735585460537,-0.999999999999995));
#10394=CARTESIAN_POINT('',(10.5993296457206,-6.46800130478792,-0.999999999999996));
#10395=CARTESIAN_POINT('Origin',(11.9508361962233,-4.21293171278112,-0.999999999999996));
#10396=CARTESIAN_POINT('',(11.8404650266211,-4.45934235565321,1.));
#10397=CARTESIAN_POINT('',(11.6956581991509,-4.12470365709515,1.));
#10398=CARTESIAN_POINT('Origin',(11.9508361962233,-4.21293171278112,1.));
#10399=CARTESIAN_POINT('',(11.8404650266211,-4.45934235565321,-0.999999999999996));
#10400=CARTESIAN_POINT('',(11.8404650266211,-4.45934235565321,-0.999999999999996));
#10401=CARTESIAN_POINT('',(11.6956581991509,-4.12470365709515,-0.999999999999996));
#10402=CARTESIAN_POINT('Origin',(11.9508361962233,-4.21293171278112,-0.999999999999996));
#10403=CARTESIAN_POINT('',(11.6956581991509,-4.12470365709515,-0.999999999999996));
#10404=CARTESIAN_POINT('Origin',(12.5487757571153,-1.63791873411964,-0.999999999999996));
#10405=CARTESIAN_POINT('',(12.4920481157737,-1.90189216972978,1.));
#10406=CARTESIAN_POINT('',(12.2808303672837,-1.6046731619638,1.));
#10407=CARTESIAN_POINT('Origin',(12.5487757571153,-1.63791873411964,1.));
#10408=CARTESIAN_POINT('',(12.4920481157737,-1.90189216972978,-0.999999999999996));
#10409=CARTESIAN_POINT('',(12.4920481157737,-1.90189216972978,-0.999999999999996));
#10410=CARTESIAN_POINT('',(12.2808303672837,-1.6046731619638,-0.999999999999996));
#10411=CARTESIAN_POINT('Origin',(12.5487757571153,-1.63791873411964,-0.999999999999996));
#10412=CARTESIAN_POINT('',(12.2808303672837,-1.6046731619638,-0.999999999999996));
#10413=CARTESIAN_POINT('Origin',(12.5487757571153,1.47608319114314,-0.999999999999996));
#10414=CARTESIAN_POINT('',(12.2808303672837,1.44283761898731,1.));
#10415=CARTESIAN_POINT('',(12.4920481157738,1.74005662675329,1.));
#10416=CARTESIAN_POINT('Origin',(12.5487757571153,1.47608319114314,1.));
#10417=CARTESIAN_POINT('',(12.2808303672837,1.44283761898731,-0.999999999999996));
#10418=CARTESIAN_POINT('',(12.2808303672837,1.44283761898731,-0.999999999999996));
#10419=CARTESIAN_POINT('',(12.4920481157738,1.74005662675329,-0.999999999999996));
#10420=CARTESIAN_POINT('Origin',(12.5487757571153,1.47608319114314,-0.999999999999996));
#10421=CARTESIAN_POINT('',(12.4920481157738,1.74005662675329,-0.999999999999996));
#10422=CARTESIAN_POINT('Origin',(9.23699064246681,8.55470779189644,-0.999999999999996));
#10423=CARTESIAN_POINT('',(9.03975952554581,8.37031721047186,1.));
#10424=CARTESIAN_POINT('',(9.03593732412206,8.73492311639068,1.));
#10425=CARTESIAN_POINT('Origin',(9.23699064246681,8.55470779189644,1.));
#10426=CARTESIAN_POINT('',(9.03975952554581,8.37031721047186,-0.999999999999996));
#10427=CARTESIAN_POINT('',(9.03975952554581,8.37031721047186,-0.999999999999996));
#10428=CARTESIAN_POINT('',(9.03593732412206,8.73492311639068,-0.999999999999996));
#10429=CARTESIAN_POINT('Origin',(9.23699064246681,8.55470779189644,-0.999999999999996));
#10430=CARTESIAN_POINT('',(9.03593732412206,8.73492311639068,-0.999999999999996));
#10431=CARTESIAN_POINT('Origin',(7.23969272277717,10.2864769967151,-0.999999999999996));
#10432=CARTESIAN_POINT('',(7.08510853652571,10.0651091368958,1.));
#10433=CARTESIAN_POINT('',(7.00556402899182,10.420952848623,1.));
#10434=CARTESIAN_POINT('Origin',(7.23969272277717,10.2864769967151,1.));
#10435=CARTESIAN_POINT('',(7.08510853652571,10.0651091368958,-0.999999999999996));
#10436=CARTESIAN_POINT('',(7.08510853652571,10.0651091368958,-0.999999999999996));
#10437=CARTESIAN_POINT('',(7.00556402899182,10.420952848623,-0.999999999999996));
#10438=CARTESIAN_POINT('Origin',(7.23969272277717,10.2864769967151,-0.999999999999996));
#10439=CARTESIAN_POINT('',(7.00556402899182,10.420952848623,-0.999999999999996));
#10440=CARTESIAN_POINT('Origin',(10.8305877470819,6.4455203116289,-0.999999999999996));
#10441=CARTESIAN_POINT('',(10.5993296457207,6.30616576181146,1.));
#10442=CARTESIAN_POINT('',(10.6713967989503,6.66359883425999,1.));
#10443=CARTESIAN_POINT('Origin',(10.8305877470819,6.44552031162891,1.));
#10444=CARTESIAN_POINT('',(10.5993296457207,6.30616576181146,-0.999999999999996));
#10445=CARTESIAN_POINT('',(10.5993296457207,6.30616576181146,-0.999999999999996));
#10446=CARTESIAN_POINT('',(10.6713967989503,6.66359883425999,-0.999999999999996));
#10447=CARTESIAN_POINT('Origin',(10.8305877470819,6.44552031162891,-0.999999999999995));
#10448=CARTESIAN_POINT('',(10.6713967989503,6.66359883425999,-0.999999999999996));
#10449=CARTESIAN_POINT('Origin',(11.9508361962234,4.05109616980463,-0.999999999999996));
#10450=CARTESIAN_POINT('',(11.695658199151,3.96286811411867,1.));
#10451=CARTESIAN_POINT('',(11.8404650266212,4.29750681267673,1.));
#10452=CARTESIAN_POINT('Origin',(11.9508361962234,4.05109616980463,1.));
#10453=CARTESIAN_POINT('',(11.695658199151,3.96286811411867,-0.999999999999996));
#10454=CARTESIAN_POINT('',(11.695658199151,3.96286811411867,-0.999999999999996));
#10455=CARTESIAN_POINT('',(11.8404650266212,4.29750681267673,-0.999999999999996));
#10456=CARTESIAN_POINT('Origin',(11.9508361962234,4.05109616980463,-0.999999999999996));
#10457=CARTESIAN_POINT('',(11.8404650266212,4.29750681267673,-0.999999999999996));
#10458=CARTESIAN_POINT('Origin',(1.56125112837913E-14,-0.080917771488119,
1.));
#10459=CARTESIAN_POINT('',(-14.3959081946537,0.26234197142012,1.));
#10460=CARTESIAN_POINT('',(-14.3959081946537,-0.424177514396259,1.));
#10461=CARTESIAN_POINT('Origin',(-1.64885466391596E-12,-0.0809177714880671,
1.00000000000058));
#10462=CARTESIAN_POINT('',(-14.3959081946537,0.262341971420116,-0.999999999999996));
#10463=CARTESIAN_POINT('',(-14.3959081946537,0.262341971420116,4.11429224827654E-15));
#10464=CARTESIAN_POINT('',(-14.3959081946537,-0.424177514396258,-0.999999999999996));
#10465=CARTESIAN_POINT('Origin',(-1.91426735574041E-12,-0.0809177714880703,
-1.00000000000057));
#10466=CARTESIAN_POINT('',(-14.3959081946537,-0.424177514396259,4.11429224827654E-15));
#10467=CARTESIAN_POINT('Origin',(1.56125112837913E-14,-0.080917771488119,
1.));
#10468=CARTESIAN_POINT('',(-9.88783448111204,-10.5494768544819,1.));
#10469=CARTESIAN_POINT('',(-9.37765107763819,-11.0088480543034,1.));
#10470=CARTESIAN_POINT('Origin',(-6.10622663543836E-13,-0.0809177714888648,
1.00000000000058));
#10471=CARTESIAN_POINT('',(-9.88783448111203,-10.5494768544819,-0.999999999999996));
#10472=CARTESIAN_POINT('',(-9.88783448111203,-10.5494768544819,4.11429224827654E-15));
#10473=CARTESIAN_POINT('',(-9.37765107763819,-11.0088480543034,-0.999999999999996));
#10474=CARTESIAN_POINT('Origin',(2.08166817117217E-13,-0.0809177714878881,
-1.00000000000057));
#10475=CARTESIAN_POINT('',(-9.37765107763819,-11.0088480543034,4.11429224827654E-15));
#10476=CARTESIAN_POINT('Origin',(1.56125112837913E-14,-0.080917771488119,
1.));
#10477=CARTESIAN_POINT('',(-11.8482973935236,-8.26491733616443,-0.999999999999996));
#10478=CARTESIAN_POINT('',(-11.4447713643493,-8.82032326715943,-0.999999999999996));
#10479=CARTESIAN_POINT('Origin',(3.06005221162309E-12,-0.0809177714858984,
-1.00000000000057));
#10480=CARTESIAN_POINT('',(-11.4447713643493,-8.82032326715942,1.));
#10481=CARTESIAN_POINT('',(-11.4447713643493,-8.82032326715943,4.11429224827654E-15));
#10482=CARTESIAN_POINT('',(-11.8482973935236,-8.26491733616442,1.));
#10483=CARTESIAN_POINT('Origin',(1.35221694952392E-12,-0.0809177714871127,
1.00000000000058));
#10484=CARTESIAN_POINT('',(-11.8482973935236,-8.26491733616443,4.11429224827654E-15));
#10485=CARTESIAN_POINT('Origin',(1.56125112837913E-14,-0.080917771488119,
1.));
#10486=CARTESIAN_POINT('',(-7.49522575478187,-12.3765101071527,1.));
#10487=CARTESIAN_POINT('',(-6.90068243987186,-12.7197698500609,1.));
#10488=CARTESIAN_POINT('Origin',(3.30031141304588E-13,-0.0809177714875715,
1.00000000000058));
#10489=CARTESIAN_POINT('',(-7.49522575478187,-12.3765101071527,-0.999999999999996));
#10490=CARTESIAN_POINT('',(-7.49522575478187,-12.3765101071527,4.11429224827654E-15));
#10491=CARTESIAN_POINT('',(-6.90068243987186,-12.7197698500609,-0.999999999999996));
#10492=CARTESIAN_POINT('Origin',(3.30031141304588E-13,-0.0809177714875715,
-1.00000000000057));
#10493=CARTESIAN_POINT('',(-6.90068243987186,-12.7197698500609,4.11429224827654E-15));
#10494=CARTESIAN_POINT('Origin',(1.56125112837913E-14,-0.080917771488119,
1.));
#10495=CARTESIAN_POINT('',(-4.7750396968842,-13.666166973957,1.));
#10496=CARTESIAN_POINT('',(-4.12212086633492,-13.8783131620438,1.));
#10497=CARTESIAN_POINT('Origin',(-7.39859562504108E-13,-0.0809177714905249,
1.00000000000058));
#10498=CARTESIAN_POINT('',(-4.7750396968842,-13.666166973957,-0.999999999999996));
#10499=CARTESIAN_POINT('',(-4.7750396968842,-13.666166973957,4.11429224827654E-15));
#10500=CARTESIAN_POINT('',(-4.12212086633494,-13.8783131620438,-0.999999999999996));
#10501=CARTESIAN_POINT('Origin',(5.34294830600857E-13,-0.0809177714868057,
-1.00000000000057));
#10502=CARTESIAN_POINT('',(-4.12212086633494,-13.8783131620438,4.11429224827654E-15));
#10503=CARTESIAN_POINT('Origin',(1.56125112837913E-14,-0.080917771488119,
1.));
#10504=CARTESIAN_POINT('',(-13.2909328553994,-5.62267776568361,-0.999999999999996));
#10505=CARTESIAN_POINT('',(-13.0117002243323,-6.24984452353429,-0.999999999999996));
#10506=CARTESIAN_POINT('Origin',(-2.78076173199082E-12,-0.0809177714893193,
-1.00000000000057));
#10507=CARTESIAN_POINT('',(-13.0117002243323,-6.24984452353429,1.));
#10508=CARTESIAN_POINT('',(-13.0117002243323,-6.24984452353429,4.11429224827654E-15));
#10509=CARTESIAN_POINT('',(-13.2909328553994,-5.62267776568361,1.));
#10510=CARTESIAN_POINT('Origin',(-2.78076173199082E-12,-0.0809177714893193,
1.00000000000058));
#10511=CARTESIAN_POINT('',(-13.2909328553994,-5.62267776568361,4.11429224827654E-15));
#10512=CARTESIAN_POINT('Origin',(1.56125112837913E-14,-0.080917771488119,
1.));
#10513=CARTESIAN_POINT('',(-14.1526907745224,-2.73823669114163,-0.999999999999996));
#10514=CARTESIAN_POINT('',(-14.009955347447,-3.40975407904992,-0.999999999999996));
#10515=CARTESIAN_POINT('Origin',(2.91433543964104E-13,-0.0809177714879744,
-1.00000000000057));
#10516=CARTESIAN_POINT('',(-14.009955347447,-3.40975407904993,1.));
#10517=CARTESIAN_POINT('',(-14.009955347447,-3.40975407904992,4.11429224827654E-15));
#10518=CARTESIAN_POINT('',(-14.1526907745224,-2.73823669114163,1.));
#10519=CARTESIAN_POINT('Origin',(-1.5256892971216E-12,-0.0809177714883608,
1.00000000000058));
#10520=CARTESIAN_POINT('',(-14.1526907745224,-2.73823669114163,4.11429224827654E-15));
#10521=CARTESIAN_POINT('Origin',(1.56125112837913E-14,-0.080917771488119,
1.));
#10522=CARTESIAN_POINT('',(-14.0099553474469,3.24791853607378,-0.999999999999996));
#10523=CARTESIAN_POINT('',(-14.1526907745224,2.57640114816549,-0.999999999999996));
#10524=CARTESIAN_POINT('Origin',(6.50521303491303E-14,-0.0809177714881221,
-1.00000000000057));
#10525=CARTESIAN_POINT('',(-14.1526907745224,2.57640114816548,1.));
#10526=CARTESIAN_POINT('',(-14.1526907745224,2.57640114816548,4.11429224827654E-15));
#10527=CARTESIAN_POINT('',(-14.0099553474469,3.24791853607378,1.));
#10528=CARTESIAN_POINT('Origin',(3.01841884819964E-13,-0.080917771488147,
1.00000000000058));
#10529=CARTESIAN_POINT('',(-14.0099553474469,3.24791853607378,4.11429224827654E-15));
#10530=CARTESIAN_POINT('Origin',(1.56125112837913E-14,-0.080917771488119,
1.));
#10531=CARTESIAN_POINT('',(-6.90068243987177,12.5579343070847,1.));
#10532=CARTESIAN_POINT('',(-7.49522575478179,12.2146745641765,1.));
#10533=CARTESIAN_POINT('Origin',(8.31799906730879E-13,-0.0809177714895326,
1.00000000000058));
#10534=CARTESIAN_POINT('',(-6.90068243987177,12.5579343070847,-0.999999999999996));
#10535=CARTESIAN_POINT('',(-6.90068243987177,12.5579343070847,4.11429224827654E-15));
#10536=CARTESIAN_POINT('',(-7.49522575478179,12.2146745641765,-0.999999999999996));
#10537=CARTESIAN_POINT('Origin',(8.31799906730879E-13,-0.0809177714895326,
-1.00000000000057));
#10538=CARTESIAN_POINT('',(-7.49522575478179,12.2146745641765,4.11429224827654E-15));
#10539=CARTESIAN_POINT('Origin',(1.56125112837913E-14,-0.080917771488119,
1.));
#10540=CARTESIAN_POINT('',(-9.37765107763812,10.8470125113272,1.));
#10541=CARTESIAN_POINT('',(-9.88783448111196,10.3876413115057,1.));
#10542=CARTESIAN_POINT('Origin',(3.41740524767431E-13,-0.0809177714884615,
1.00000000000058));
#10543=CARTESIAN_POINT('',(-9.37765107763812,10.8470125113272,-0.999999999999996));
#10544=CARTESIAN_POINT('',(-9.37765107763812,10.8470125113272,4.11429224827654E-15));
#10545=CARTESIAN_POINT('',(-9.88783448111196,10.3876413115057,-0.999999999999996));
#10546=CARTESIAN_POINT('Origin',(1.16226472890446E-13,-0.0809177714881162,
-1.00000000000057));
#10547=CARTESIAN_POINT('',(-9.88783448111196,10.3876413115057,4.11429224827654E-15));
#10548=CARTESIAN_POINT('Origin',(1.56125112837913E-14,-0.080917771488119,
1.));
#10549=CARTESIAN_POINT('',(-13.0117002243322,6.08800898055815,-0.999999999999996));
#10550=CARTESIAN_POINT('',(-13.2909328553993,5.46084222270746,-0.999999999999996));
#10551=CARTESIAN_POINT('Origin',(-7.91033905045424E-13,-0.0809177714877533,
-1.00000000000057));
#10552=CARTESIAN_POINT('',(-13.2909328553993,5.46084222270746,1.));
#10553=CARTESIAN_POINT('',(-13.2909328553993,5.46084222270746,4.11429224827654E-15));
#10554=CARTESIAN_POINT('',(-13.0117002243322,6.08800898055815,1.));
#10555=CARTESIAN_POINT('Origin',(-5.57713597526543E-13,-0.0809177714879142,
1.00000000000058));
#10556=CARTESIAN_POINT('',(-13.0117002243322,6.08800898055815,4.11429224827654E-15));
#10557=CARTESIAN_POINT('Origin',(1.56125112837913E-14,-0.080917771488119,
1.));
#10558=CARTESIAN_POINT('',(-11.4447713643492,8.65848772418326,-0.999999999999996));
#10559=CARTESIAN_POINT('',(-11.8482973935235,8.10308179318827,-0.999999999999996));
#10560=CARTESIAN_POINT('Origin',(-9.2374025095765E-13,-0.0809177714874276,
-1.00000000000057));
#10561=CARTESIAN_POINT('',(-11.8482973935235,8.10308179318827,1.));
#10562=CARTESIAN_POINT('',(-11.8482973935235,8.10308179318827,4.11429224827654E-15));
#10563=CARTESIAN_POINT('',(-11.4447713643492,8.65848772418327,1.));
#10564=CARTESIAN_POINT('Origin',(-9.2374025095765E-13,-0.0809177714874276,
1.00000000000058));
#10565=CARTESIAN_POINT('',(-11.4447713643492,8.65848772418326,4.11429224827654E-15));
#10566=CARTESIAN_POINT('Origin',(1.56125112837913E-14,-0.080917771488119,
1.));
#10567=CARTESIAN_POINT('',(-4.12212086633484,13.7164776190675,-0.999999999999996));
#10568=CARTESIAN_POINT('',(-4.7750396968841,13.5043314309807,-0.999999999999996));
#10569=CARTESIAN_POINT('Origin',(5.96311194867027E-13,-0.0809177714895457,
-1.00000000000057));
#10570=CARTESIAN_POINT('',(-4.7750396968841,13.5043314309807,1.));
#10571=CARTESIAN_POINT('',(-4.7750396968841,13.5043314309807,4.11429224827654E-15));
#10572=CARTESIAN_POINT('',(-4.12212086633484,13.7164776190676,1.));
#10573=CARTESIAN_POINT('Origin',(5.23886489744996E-13,-0.0809177714893947,
1.00000000000058));
#10574=CARTESIAN_POINT('',(-4.12212086633484,13.7164776190675,4.11429224827654E-15));
#10575=CARTESIAN_POINT('Origin',(1.56125112837913E-14,-0.080917771488119,
1.));
#10576=CARTESIAN_POINT('',(-1.16340283080869,14.2720085452344,-0.999999999999996));
#10577=CARTESIAN_POINT('',(-1.84616149104994,14.2002477183787,-0.999999999999996));
#10578=CARTESIAN_POINT('Origin',(4.23489368572838E-13,-0.0809177714917566,
-1.00000000000057));
#10579=CARTESIAN_POINT('',(-1.84616149104994,14.2002477183787,1.));
#10580=CARTESIAN_POINT('',(-1.84616149104994,14.2002477183787,4.11429224827654E-15));
#10581=CARTESIAN_POINT('',(-1.16340283080868,14.2720085452344,1.));
#10582=CARTESIAN_POINT('Origin',(4.41378704418849E-13,-0.0809177714920367,
1.00000000000058));
#10583=CARTESIAN_POINT('',(-1.16340283080869,14.2720085452344,4.11429224827654E-15));
#10584=CARTESIAN_POINT('Origin',(1.56125112837913E-14,-0.080917771488119,
1.));
#10585=CARTESIAN_POINT('',(1.16340283080872,14.2720085452344,-0.999999999999996));
#10586=CARTESIAN_POINT('Origin',(-1.63714528045311E-14,-0.0809177714885716,
-1.00000000000057));
#10587=CARTESIAN_POINT('',(1.16340283080872,14.2720085452344,1.));
#10588=CARTESIAN_POINT('',(1.16340283080872,14.2720085452344,4.11429224827654E-15));
#10589=CARTESIAN_POINT('Origin',(-2.37440275774325E-14,-0.0809177714887312,
1.00000000000058));
#10590=CARTESIAN_POINT('Origin',(1.56125112837913E-14,-0.080917771488119,
1.));
#10591=CARTESIAN_POINT('',(4.12212086633506,13.7164776190675,-0.999999999999996));
#10592=CARTESIAN_POINT('Origin',(2.3115190317391E-13,-0.0809177714871977,
-1.00000000000057));
#10593=CARTESIAN_POINT('',(4.12212086633506,13.7164776190675,1.));
#10594=CARTESIAN_POINT('',(4.12212086633506,13.7164776190675,4.11429224827654E-15));
#10595=CARTESIAN_POINT('Origin',(9.15066633577766E-14,-0.0809177714876609,
1.00000000000058));
#10596=CARTESIAN_POINT('Origin',(1.56125112837913E-14,-0.080917771488119,
1.));
#10597=CARTESIAN_POINT('',(4.12212086633478,-13.8783131620438,1.));
#10598=CARTESIAN_POINT('Origin',(-4.75747913286639E-13,-0.0809177714867961,
1.00000000000058));
#10599=CARTESIAN_POINT('',(4.12212086633479,-13.8783131620438,-0.999999999999996));
#10600=CARTESIAN_POINT('',(4.12212086633479,-13.8783131620438,4.11429224827654E-15));
#10601=CARTESIAN_POINT('Origin',(-4.75747913286639E-13,-0.0809177714867961,
-1.00000000000057));
#10602=CARTESIAN_POINT('Origin',(1.56125112837913E-14,-0.080917771488119,
1.));
#10603=CARTESIAN_POINT('',(6.90068243987172,-12.719769850061,1.));
#10604=CARTESIAN_POINT('',(7.49522575478174,-12.3765101071528,1.));
#10605=CARTESIAN_POINT('Origin',(-1.02955838299224E-12,-0.0809177714864821,
1.00000000000058));
#10606=CARTESIAN_POINT('',(6.90068243987173,-12.719769850061,-0.999999999999996));
#10607=CARTESIAN_POINT('',(6.90068243987173,-12.719769850061,4.11429224827654E-15));
#10608=CARTESIAN_POINT('',(7.49522575478174,-12.3765101071528,-0.999999999999996));
#10609=CARTESIAN_POINT('Origin',(-3.17020715234761E-13,-0.0809177714876869,
-1.00000000000057));
#10610=CARTESIAN_POINT('',(7.49522575478174,-12.3765101071528,4.11429224827654E-15));
#10611=CARTESIAN_POINT('Origin',(1.56125112837913E-14,-0.080917771488119,
1.));
#10612=CARTESIAN_POINT('',(11.4447713643492,-8.82032326715959,1.));
#10613=CARTESIAN_POINT('',(11.8482973935235,-8.26491733616459,1.));
#10614=CARTESIAN_POINT('Origin',(-6.05418493115906E-13,-0.0809177714877095,
1.00000000000058));
#10615=CARTESIAN_POINT('',(11.4447713643492,-8.82032326715958,-0.999999999999996));
#10616=CARTESIAN_POINT('',(11.4447713643492,-8.82032326715958,4.11429224827654E-15));
#10617=CARTESIAN_POINT('',(11.8482973935235,-8.26491733616459,-0.999999999999996));
#10618=CARTESIAN_POINT('Origin',(-8.26595736302949E-13,-0.0809177714874432,
-1.00000000000057));
#10619=CARTESIAN_POINT('',(11.8482973935235,-8.26491733616459,4.11429224827654E-15));
#10620=CARTESIAN_POINT('Origin',(1.56125112837913E-14,-0.080917771488119,
1.));
#10621=CARTESIAN_POINT('',(9.37765107763808,-11.0088480543035,-0.999999999999996));
#10622=CARTESIAN_POINT('',(9.88783448111192,-10.549476854482,-0.999999999999996));
#10623=CARTESIAN_POINT('Origin',(-2.78423117894278E-13,-0.0809177714878413,
-1.00000000000057));
#10624=CARTESIAN_POINT('',(9.88783448111192,-10.549476854482,1.));
#10625=CARTESIAN_POINT('',(9.88783448111192,-10.549476854482,4.11429224827654E-15));
#10626=CARTESIAN_POINT('',(9.37765107763808,-11.0088480543035,1.));
#10627=CARTESIAN_POINT('Origin',(-2.78423117894278E-13,-0.0809177714878413,
1.00000000000058));
#10628=CARTESIAN_POINT('',(9.37765107763808,-11.0088480543035,4.11429224827654E-15));
#10629=CARTESIAN_POINT('Origin',(1.56125112837913E-14,-0.080917771488119,
1.));
#10630=CARTESIAN_POINT('',(13.0117002243322,-6.24984452353448,1.));
#10631=CARTESIAN_POINT('',(13.2909328553993,-5.62267776568378,1.));
#10632=CARTESIAN_POINT('Origin',(3.37403716077489E-13,-0.0809177714882576,
1.00000000000058));
#10633=CARTESIAN_POINT('',(13.0117002243322,-6.24984452353447,-0.999999999999996));
#10634=CARTESIAN_POINT('',(13.0117002243322,-6.24984452353448,4.11429224827654E-15));
#10635=CARTESIAN_POINT('',(13.2909328553993,-5.62267776568379,-0.999999999999996));
#10636=CARTESIAN_POINT('Origin',(3.37403716077489E-13,-0.0809177714882576,
-1.00000000000057));
#10637=CARTESIAN_POINT('',(13.2909328553993,-5.62267776568379,4.11429224827654E-15));
#10638=CARTESIAN_POINT('Origin',(1.56125112837913E-14,-0.080917771488119,
1.));
#10639=CARTESIAN_POINT('',(14.009955347447,-3.40975407905011,1.));
#10640=CARTESIAN_POINT('',(14.1526907745224,-2.73823669114181,1.));
#10641=CARTESIAN_POINT('Origin',(-2.28549817959944E-12,-0.0809177714875657,
1.00000000000058));
#10642=CARTESIAN_POINT('',(14.009955347447,-3.40975407905011,-0.999999999999996));
#10643=CARTESIAN_POINT('',(14.009955347447,-3.40975407905011,4.11429224827654E-15));
#10644=CARTESIAN_POINT('',(14.1526907745224,-2.73823669114182,-0.999999999999996));
#10645=CARTESIAN_POINT('Origin',(-2.28549817959944E-12,-0.0809177714875657,
-1.00000000000057));
#10646=CARTESIAN_POINT('',(14.1526907745224,-2.73823669114182,4.11429224827654E-15));
#10647=CARTESIAN_POINT('Origin',(1.56125112837913E-14,-0.080917771488119,
1.));
#10648=CARTESIAN_POINT('',(14.3959081946538,-0.424177514396453,1.));
#10649=CARTESIAN_POINT('',(14.3959081946538,0.262341971419921,1.));
#10650=CARTESIAN_POINT('Origin',(1.59681295963665E-12,-0.0809177714880441,
1.00000000000058));
#10651=CARTESIAN_POINT('',(14.3959081946537,-0.42417751439645,-0.999999999999996));
#10652=CARTESIAN_POINT('',(14.3959081946537,-0.42417751439645,4.11429224827654E-15));
#10653=CARTESIAN_POINT('',(14.3959081946538,0.262341971419921,-0.999999999999996));
#10654=CARTESIAN_POINT('Origin',(1.59681295963665E-12,-0.0809177714880441,
-1.00000000000057));
#10655=CARTESIAN_POINT('',(14.3959081946538,0.262341971419922,4.11429224827654E-15));
#10656=CARTESIAN_POINT('Origin',(1.56125112837913E-14,-0.080917771488119,
1.));
#10657=CARTESIAN_POINT('',(14.1526907745224,2.57640114816529,1.));
#10658=CARTESIAN_POINT('',(14.009955347447,3.24791853607358,1.));
#10659=CARTESIAN_POINT('Origin',(-2.38958158815805E-12,-0.0809177714885389,
1.00000000000058));
#10660=CARTESIAN_POINT('',(14.1526907745224,2.57640114816529,-0.999999999999996));
#10661=CARTESIAN_POINT('',(14.1526907745224,2.57640114816529,4.11429224827654E-15));
#10662=CARTESIAN_POINT('',(14.009955347447,3.24791853607358,-0.999999999999996));
#10663=CARTESIAN_POINT('Origin',(1.04083408558608E-14,-0.0809177714880989,
-1.00000000000057));
#10664=CARTESIAN_POINT('',(14.009955347447,3.24791853607358,4.11429224827654E-15));
#10665=CARTESIAN_POINT('Origin',(1.56125112837913E-14,-0.080917771488119,
1.));
#10666=CARTESIAN_POINT('',(9.88783448111214,10.3876413115056,1.));
#10667=CARTESIAN_POINT('',(9.3776510776383,10.8470125113271,1.));
#10668=CARTESIAN_POINT('Origin',(-2.56739074444567E-13,-0.0809177714883591,
1.00000000000058));
#10669=CARTESIAN_POINT('',(9.88783448111214,10.3876413115056,-0.999999999999996));
#10670=CARTESIAN_POINT('',(9.88783448111214,10.3876413115056,4.11429224827654E-15));
#10671=CARTESIAN_POINT('',(9.3776510776383,10.8470125113271,-0.999999999999996));
#10672=CARTESIAN_POINT('Origin',(7.92768628521401E-13,-0.0809177714871318,
-1.00000000000057));
#10673=CARTESIAN_POINT('',(9.3776510776383,10.8470125113271,4.11429224827654E-15));
#10674=CARTESIAN_POINT('Origin',(1.56125112837913E-14,-0.080917771488119,
1.));
#10675=CARTESIAN_POINT('',(7.49522575478199,12.2146745641764,-0.999999999999996));
#10676=CARTESIAN_POINT('',(6.90068243987198,12.5579343070846,-0.999999999999996));
#10677=CARTESIAN_POINT('Origin',(-1.11586087592208E-12,-0.0809177714900123,
-1.00000000000057));
#10678=CARTESIAN_POINT('',(6.90068243987197,12.5579343070846,1.));
#10679=CARTESIAN_POINT('',(6.90068243987198,12.5579343070846,4.11429224827654E-15));
#10680=CARTESIAN_POINT('',(7.49522575478199,12.2146745641764,1.));
#10681=CARTESIAN_POINT('Origin',(-1.04864034122798E-12,-0.0809177714898978,
1.00000000000058));
#10682=CARTESIAN_POINT('',(7.49522575478199,12.2146745641764,4.11429224827654E-15));
#10683=CARTESIAN_POINT('Origin',(1.56125112837913E-14,-0.080917771488119,
1.));
#10684=CARTESIAN_POINT('',(11.8482973935237,8.1030817931881,-0.999999999999996));
#10685=CARTESIAN_POINT('',(11.4447713643494,8.65848772418311,-0.999999999999996));
#10686=CARTESIAN_POINT('Origin',(-2.41386771682173E-12,-0.0809177714898883,
-1.00000000000057));
#10687=CARTESIAN_POINT('',(11.4447713643494,8.65848772418311,1.));
#10688=CARTESIAN_POINT('',(11.4447713643494,8.65848772418311,4.11429224827654E-15));
#10689=CARTESIAN_POINT('',(11.8482973935237,8.1030817931881,1.));
#10690=CARTESIAN_POINT('Origin',(-1.56385321359309E-12,-0.0809177714893453,
1.00000000000058));
#10691=CARTESIAN_POINT('',(11.8482973935237,8.1030817931881,4.11429224827654E-15));
#10692=CARTESIAN_POINT('Origin',(1.56125112837913E-14,-0.080917771488119,
1.));
#10693=CARTESIAN_POINT('',(13.2909328553994,5.46084222270728,-0.999999999999996));
#10694=CARTESIAN_POINT('',(13.0117002243324,6.08800898055796,-0.999999999999996));
#10695=CARTESIAN_POINT('Origin',(1.32879818259823E-12,-0.080917771487513,
-1.00000000000057));
#10696=CARTESIAN_POINT('',(13.0117002243324,6.08800898055796,1.));
#10697=CARTESIAN_POINT('',(13.0117002243324,6.08800898055796,4.11429224827654E-15));
#10698=CARTESIAN_POINT('',(13.2909328553994,5.46084222270728,1.));
#10699=CARTESIAN_POINT('Origin',(8.4741241801467E-13,-0.080917771487827,
1.00000000000058));
#10700=CARTESIAN_POINT('',(13.2909328553994,5.46084222270728,4.11429224827654E-15));
#10701=CARTESIAN_POINT('Origin',(1.56125112837913E-14,-0.080917771488119,
1.));
#10702=CARTESIAN_POINT('',(-1.84616149105004,-14.362083261355,1.));
#10703=CARTESIAN_POINT('',(-1.16340283080869,-14.4338440882107,1.));
#10704=CARTESIAN_POINT('Origin',(-1.5710089479315E-13,-0.0809177714894745,
1.00000000000058));
#10705=CARTESIAN_POINT('',(-1.84616149105004,-14.362083261355,-0.999999999999996));
#10706=CARTESIAN_POINT('',(-1.84616149105004,-14.362083261355,4.11429224827654E-15));
#10707=CARTESIAN_POINT('',(-1.16340283080869,-14.4338440882107,-0.999999999999996));
#10708=CARTESIAN_POINT('Origin',(-1.5710089479315E-13,-0.0809177714894745,
-1.00000000000057));
#10709=CARTESIAN_POINT('',(-1.16340283080869,-14.4338440882107,4.11429224827654E-15));
#10710=CARTESIAN_POINT('Origin',(1.61979340522206E-14,-0.0809177714881199,
-0.999999999999996));
#10711=CARTESIAN_POINT('',(-9.03593732412197,-8.89675865936698,-0.999999999999996));
#10712=CARTESIAN_POINT('Origin',(-6.29005919429158,-11.3580426722998,-1.));
#10713=CARTESIAN_POINT('',(-9.03975952554573,-8.53215275344816,-0.999999999999996));
#10714=CARTESIAN_POINT('Origin',(-9.23699064246671,-8.71654333487274,-0.999999999999995));
#10715=CARTESIAN_POINT('',(-9.349850403976,-8.18776194312912,-0.999999999999996));
#10716=CARTESIAN_POINT('Origin',(-1.94202293135604E-12,-0.0809177714900912,
-0.999999999999996));
#10717=CARTESIAN_POINT('',(-9.71205943175173,-8.14584898508068,-0.999999999999996));
#10718=CARTESIAN_POINT('Origin',(-9.55384714006274,-8.36463854323765,-0.999999999999996));
#10719=CARTESIAN_POINT('Origin',(-11.8728378521018,-5.15773882741439,-0.999999999999996));
#10720=CARTESIAN_POINT('',(-10.6713967989502,-6.82543437723631,-0.999999999999996));
#10721=CARTESIAN_POINT('Origin',(-8.4972524150608,-9.80383359396352,-0.999999999999996));
#10722=CARTESIAN_POINT('',(-10.5993296457206,-6.46800130478777,-0.999999999999996));
#10723=CARTESIAN_POINT('Origin',(-10.8305877470818,-6.60735585460522,-0.999999999999996));
#10724=CARTESIAN_POINT('',(-10.8310414187911,-6.06666474111783,-0.999999999999996));
#10725=CARTESIAN_POINT('Origin',(1.26721549920106E-12,-0.0809177714874432,
-0.999999999999996));
#10726=CARTESIAN_POINT('',(-11.176621116299,-5.95036019036879,-0.999999999999996));
#10727=CARTESIAN_POINT('Origin',(-11.0673550497465,-6.19726285681884,-0.999999999999996));
#10728=CARTESIAN_POINT('Origin',(-12.6689183086518,-2.57829631406167,-1.));
#10729=CARTESIAN_POINT('',(-11.8404650266211,-4.45934235565306,-0.999999999999996));
#10730=CARTESIAN_POINT('Origin',(-10.3330749309508,-7.82468643845863,-0.999999999999996));
#10731=CARTESIAN_POINT('',(-11.6956581991509,-4.12470365709499,-0.999999999999996));
#10732=CARTESIAN_POINT('Origin',(-11.9508361962233,-4.21293171278095,-0.999999999999996));
#10733=CARTESIAN_POINT('',(-11.838863950502,-3.68396167373302,-0.999999999999996));
#10734=CARTESIAN_POINT('Origin',(9.35449634420493E-12,-0.0809177714850636,
-0.999999999999996));
#10735=CARTESIAN_POINT('',(-12.1527108266856,-3.49834859724226,-0.999999999999996));
#10736=CARTESIAN_POINT('Origin',(-12.0971664366948,-3.76257354069109,-0.999999999999996));
#10737=CARTESIAN_POINT('Origin',(-12.9113062428988,0.110293625353355,-1.));
#10738=CARTESIAN_POINT('',(-12.4920481157737,-1.90189216972961,-0.999999999999996));
#10739=CARTESIAN_POINT('Origin',(-11.7172924887636,-5.50709943348233,-0.999999999999996));
#10740=CARTESIAN_POINT('',(-12.2808303672837,-1.60467316196364,-0.999999999999996));
#10741=CARTESIAN_POINT('Origin',(-12.5487757571153,-1.63791873411946,-0.999999999999995));
#10742=CARTESIAN_POINT('',(-12.3292713184038,-1.14378829849724,-0.999999999999996));
#10743=CARTESIAN_POINT('Origin',(5.0558515707344E-12,-0.0809177714875954,
-0.999999999999996));
#10744=CARTESIAN_POINT('',(-12.5976687587696,-0.896978878377764,-0.999999999999996));
#10745=CARTESIAN_POINT('Origin',(-12.5982736017144,-1.16697820090472,-0.999999999999995));
#10746=CARTESIAN_POINT('Origin',(-12.5894081390099,2.79052670919229,-0.999999999999996));
#10747=CARTESIAN_POINT('',(-12.5976687587696,0.735143335401609,-0.999999999999996));
#10748=CARTESIAN_POINT('Origin',(-12.5894081390099,-2.95236225216844,-0.999999999999996));
#10749=CARTESIAN_POINT('',(-12.3292713184038,0.981952755521089,-0.999999999999996));
#10750=CARTESIAN_POINT('Origin',(-12.5982736017144,1.00514265792856,-0.999999999999996));
#10751=CARTESIAN_POINT('',(-12.2808303672836,1.44283761898748,-0.999999999999996));
#10752=CARTESIAN_POINT('Origin',(-2.37310171513627E-12,-0.0809177714879208,
-0.999999999999996));
#10753=CARTESIAN_POINT('',(-12.4920481157737,1.74005662675346,-0.999999999999996));
#10754=CARTESIAN_POINT('Origin',(-12.5487757571153,1.47608319114332,-0.999999999999996));
#10755=CARTESIAN_POINT('Origin',(-11.7172924887636,5.3452638905062,-1.));
#10756=CARTESIAN_POINT('',(-12.1527108266856,3.3365130542661,-0.999999999999996));
#10757=CARTESIAN_POINT('Origin',(-12.9113062428988,-0.272129168329482,-1.));
#10758=CARTESIAN_POINT('',(-11.838863950502,3.52212613075686,-0.999999999999996));
#10759=CARTESIAN_POINT('Origin',(-12.0971664366947,3.60073799771494,-0.999999999999996));
#10760=CARTESIAN_POINT('',(-11.6956581991509,3.96286811411883,-0.999999999999996));
#10761=CARTESIAN_POINT('Origin',(4.26828711264093E-12,-0.080917771489527,
-0.999999999999996));
#10762=CARTESIAN_POINT('',(-11.8404650266211,4.29750681267689,-0.999999999999996));
#10763=CARTESIAN_POINT('Origin',(-11.9508361962233,4.0510961698048,-0.999999999999996));
#10764=CARTESIAN_POINT('Origin',(-10.3330749309508,7.66285089548245,-0.999999999999996));
#10765=CARTESIAN_POINT('',(-11.176621116299,5.78852464739262,-0.999999999999996));
#10766=CARTESIAN_POINT('Origin',(-12.6689183086518,2.4164607710855,-1.));
#10767=CARTESIAN_POINT('',(-10.8310414187911,5.90482919814167,-0.999999999999996));
#10768=CARTESIAN_POINT('Origin',(-11.0673550497465,6.03542731384268,-0.999999999999996));
#10769=CARTESIAN_POINT('',(-10.5993296457206,6.30616576181161,-0.999999999999996));
#10770=CARTESIAN_POINT('Origin',(-1.49966844498195E-12,-0.0809177714873426,
-0.999999999999996));
#10771=CARTESIAN_POINT('',(-10.6713967989501,6.66359883426014,-0.999999999999996));
#10772=CARTESIAN_POINT('Origin',(-10.8305877470818,6.44552031162906,-0.999999999999996));
#10773=CARTESIAN_POINT('Origin',(-8.49725241506071,9.64199805098735,-0.999999999999996));
#10774=CARTESIAN_POINT('',(-9.71205943175167,7.98401344210451,-0.999999999999996));
#10775=CARTESIAN_POINT('Origin',(-11.8728378521018,4.99590328443823,-1.));
#10776=CARTESIAN_POINT('',(-9.34985040397594,8.02592640015294,-0.999999999999996));
#10777=CARTESIAN_POINT('Origin',(-9.55384714006268,8.20280300026148,-0.999999999999995));
#10778=CARTESIAN_POINT('',(-9.03975952554566,8.37031721047198,-0.999999999999996));
#10779=CARTESIAN_POINT('Origin',(-2.06258621293642E-12,-0.0809177714861846,
-0.999999999999996));
#10780=CARTESIAN_POINT('',(-9.03593732412191,8.7349231163908,-0.999999999999996));
#10781=CARTESIAN_POINT('Origin',(-9.23699064246666,8.55470779189656,-0.999999999999996));
#10782=CARTESIAN_POINT('Origin',(-6.29005919429155,11.1962071293236,-1.));
#10783=CARTESIAN_POINT('',(-7.82303414640506,9.82702604294875,-0.999999999999996));
#10784=CARTESIAN_POINT('Origin',(-10.557857409218,7.35346435635671,-0.999999999999996));
#10785=CARTESIAN_POINT('',(-7.46002606094707,9.79271561090918,-0.999999999999996));
#10786=CARTESIAN_POINT('Origin',(-7.62279026591319,10.0081403392524,-0.999999999999996));
#10787=CARTESIAN_POINT('',(-7.08510853652553,10.0651091368959,-0.999999999999996));
#10788=CARTESIAN_POINT('Origin',(4.36716635077161E-13,-0.080917771488739,
-0.999999999999996));
#10789=CARTESIAN_POINT('',(-7.00556402899164,10.4209528486231,-0.999999999999996));
#10790=CARTESIAN_POINT('Origin',(-7.239692722777,10.2864769967152,-0.999999999999996));
#10791=CARTESIAN_POINT('Origin',(-3.80796020367909,12.2575517358452,-0.999999999999996));
#10792=CARTESIAN_POINT('',(-5.5921047297778,11.2370139555128,-0.999999999999996));
#10793=CARTESIAN_POINT('Origin',(-8.78144793533072,9.38610725516491,-1.));
#10794=CARTESIAN_POINT('',(-5.24416278187814,11.1279796639051,-0.999999999999996));
#10795=CARTESIAN_POINT('Origin',(-5.3585808789373,11.3725374261318,-0.999999999999996));
#10796=CARTESIAN_POINT('',(-4.82080430633644,11.3164710013847,-0.999999999999996));
#10797=CARTESIAN_POINT('Origin',(-2.89265139619133E-13,-0.0809177714872558,
-0.999999999999996));
#10798=CARTESIAN_POINT('',(-4.66901396936854,11.6480004411903,-0.999999999999996));
#10799=CARTESIAN_POINT('Origin',(-4.92598549120196,11.5651413018838,-0.999999999999996));
#10800=CARTESIAN_POINT('Origin',(-1.15943507954541,12.7796460183509,-1.));
#10801=CARTESIAN_POINT('',(-3.11677350256359,12.1523539421449,-0.999999999999996));
#10802=CARTESIAN_POINT('Origin',(-6.62124704860712,11.0049957324822,-1.));
#10803=CARTESIAN_POINT('',(-2.79910442495618,11.9733611127169,-0.999999999999996));
#10804=CARTESIAN_POINT('Origin',(-2.86017579422795,12.2363635610995,-0.999999999999996));
#10805=CARTESIAN_POINT('',(-2.34580779517484,12.0697122857598,-0.999999999999996));
#10806=CARTESIAN_POINT('Origin',(-1.83013326715553E-13,-0.0809177714870919,
-0.999999999999996));
#10807=CARTESIAN_POINT('',(-2.12840559486928,12.3624380262694,-0.999999999999996));
#10808=CARTESIAN_POINT('Origin',(-2.39698905616047,12.3348169415543,-0.999999999999996));
#10809=CARTESIAN_POINT('Origin',(1.53976292115111,12.7396719514087,-0.999999999999996));
#10810=CARTESIAN_POINT('',(-0.505224317348839,12.5330412531408,-0.999999999999996));
#10811=CARTESIAN_POINT('Origin',(-4.17166589359098,12.1393765935609,-0.999999999999996));
#10812=CARTESIAN_POINT('',(-0.231711773070462,12.2919127314413,-0.999999999999996));
#10813=CARTESIAN_POINT('Origin',(-0.236767302664724,12.5618653969598,-0.999999999999996));
#10814=CARTESIAN_POINT('',(0.231711773070499,12.2919127314413,-0.999999999999996));
#10815=CARTESIAN_POINT('Origin',(1.82145964977565E-14,-0.0809177714804904,
-0.999999999999996));
#10816=CARTESIAN_POINT('',(0.505224317348871,12.5330412531408,-0.999999999999996));
#10817=CARTESIAN_POINT('Origin',(0.236767302664761,12.5618653969598,-0.999999999999996));
#10818=CARTESIAN_POINT('Origin',(4.17166589359101,12.1393765935609,-0.999999999999996));
#10819=CARTESIAN_POINT('',(2.79910442495637,11.9733611127168,-0.999999999999996));
#10820=CARTESIAN_POINT('Origin',(9.63855731339613E-13,-0.0809177714833623,
-0.999999999999996));
#10821=CARTESIAN_POINT('',(3.11677350256379,12.1523539421449,-0.999999999999996));
#10822=CARTESIAN_POINT('Origin',(2.86017579422815,12.2363635610995,-0.999999999999995));
#10823=CARTESIAN_POINT('Origin',(6.62124704860725,11.0049957324821,-0.999999999999996));
#10824=CARTESIAN_POINT('',(5.24416278187833,11.127979663905,-0.999999999999996));
#10825=CARTESIAN_POINT('Origin',(-9.87925019568792E-13,-0.0809177714904624,
-0.999999999999996));
#10826=CARTESIAN_POINT('',(5.59210472977799,11.2370139555127,-0.999999999999996));
#10827=CARTESIAN_POINT('Origin',(5.35858087893749,11.3725374261318,-0.999999999999996));
#10828=CARTESIAN_POINT('Origin',(8.78144793533089,9.38610725516478,-1.));
#10829=CARTESIAN_POINT('Origin',(3.80796020367927,12.2575517358452,-0.999999999999996));
#10830=CARTESIAN_POINT('',(7.46002606094724,9.79271561090908,-0.999999999999996));
#10831=CARTESIAN_POINT('Origin',(-7.51135265097957E-13,-0.0809177714892022,
-0.999999999999996));
#10832=CARTESIAN_POINT('',(7.82303414640522,9.82702604294864,-0.999999999999996));
#10833=CARTESIAN_POINT('Origin',(7.62279026591336,10.0081403392523,-0.999999999999996));
#10834=CARTESIAN_POINT('Origin',(10.5578574092182,7.35346435635655,-1.));
#10835=CARTESIAN_POINT('Origin',(6.29005919429175,11.1962071293235,-0.999999999999996));
#10836=CARTESIAN_POINT('',(9.34985040397608,8.02592640015281,-0.999999999999996));
#10837=CARTESIAN_POINT('Origin',(1.21430643318376E-14,-0.080917771488098,
-0.999999999999996));
#10838=CARTESIAN_POINT('',(9.71205943175181,7.98401344210438,-0.999999999999996));
#10839=CARTESIAN_POINT('Origin',(9.55384714006283,8.20280300026134,-0.999999999999995));
#10840=CARTESIAN_POINT('Origin',(11.8728378521019,4.99590328443808,-0.999999999999996));
#10841=CARTESIAN_POINT('Origin',(8.49725241506087,9.64199805098723,-1.));
#10842=CARTESIAN_POINT('',(10.8310414187912,5.90482919814151,-0.999999999999996));
#10843=CARTESIAN_POINT('Origin',(-4.47558656802016E-13,-0.0809177714884237,
-0.999999999999996));
#10844=CARTESIAN_POINT('',(11.1766211162991,5.78852464739247,-0.999999999999996));
#10845=CARTESIAN_POINT('Origin',(11.0673550497466,6.03542731384252,-0.999999999999996));
#10846=CARTESIAN_POINT('Origin',(12.6689183086518,2.41646077108533,-1.));
#10847=CARTESIAN_POINT('Origin',(10.3330749309509,7.66285089548231,-0.999999999999996));
#10848=CARTESIAN_POINT('',(11.838863950502,3.5221261307567,-0.999999999999996));
#10849=CARTESIAN_POINT('Origin',(1.47104550762833E-12,-0.0809177714876732,
-0.999999999999996));
#10850=CARTESIAN_POINT('',(12.1527108266857,3.33651305426593,-0.999999999999996));
#10851=CARTESIAN_POINT('Origin',(12.0971664366948,3.60073799771477,-0.999999999999996));
#10852=CARTESIAN_POINT('Origin',(12.9113062428988,-0.272129168329659,-0.999999999999996));
#10853=CARTESIAN_POINT('Origin',(11.7172924887637,5.345263890506,-1.));
#10854=CARTESIAN_POINT('',(12.3292713184039,0.981952755520918,-0.999999999999996));
#10855=CARTESIAN_POINT('Origin',(-1.40512601554121E-12,-0.0809177714882771,
-0.999999999999996));
#10856=CARTESIAN_POINT('',(12.5976687587696,0.735143335401439,-0.999999999999996));
#10857=CARTESIAN_POINT('Origin',(12.5982736017145,1.00514265792839,-0.999999999999996));
#10858=CARTESIAN_POINT('Origin',(12.5894081390099,-2.95236225216863,-1.));
#10859=CARTESIAN_POINT('',(12.5976687587696,-0.896978878377931,-0.999999999999996));
#10860=CARTESIAN_POINT('Origin',(12.58940813901,2.79052670919211,-0.999999999999996));
#10861=CARTESIAN_POINT('',(12.3292713184038,-1.14378829849741,-0.999999999999996));
#10862=CARTESIAN_POINT('Origin',(12.5982736017145,-1.16697820090489,-0.999999999999996));
#10863=CARTESIAN_POINT('Origin',(-5.25534477047174E-12,-0.08091777148747,
-0.999999999999996));
#10864=CARTESIAN_POINT('Origin',(11.7172924887636,-5.50709943348249,-0.999999999999996));
#10865=CARTESIAN_POINT('',(12.1527108266856,-3.49834859724242,-0.999999999999996));
#10866=CARTESIAN_POINT('Origin',(12.9113062428988,0.110293625353176,-1.));
#10867=CARTESIAN_POINT('',(11.838863950502,-3.68396167373318,-0.999999999999996));
#10868=CARTESIAN_POINT('Origin',(12.0971664366947,-3.76257354069125,-0.999999999999996));
#10869=CARTESIAN_POINT('Origin',(-2.20223145275256E-12,-0.0809177714873727,
-0.999999999999996));
#10870=CARTESIAN_POINT('Origin',(10.3330749309508,-7.82468643845877,-1.));
#10871=CARTESIAN_POINT('',(11.176621116299,-5.95036019036894,-0.999999999999996));
#10872=CARTESIAN_POINT('Origin',(12.6689183086518,-2.57829631406186,-0.999999999999996));
#10873=CARTESIAN_POINT('',(10.8310414187911,-6.06666474111799,-0.999999999999996));
#10874=CARTESIAN_POINT('Origin',(11.0673550497465,-6.197262856819,-0.999999999999996));
#10875=CARTESIAN_POINT('Origin',(2.35835656559047E-12,-0.0809177714894533,
-0.999999999999996));
#10876=CARTESIAN_POINT('Origin',(8.49725241506068,-9.80383359396365,-0.999999999999996));
#10877=CARTESIAN_POINT('',(9.71205943175165,-8.14584898508081,-0.999999999999996));
#10878=CARTESIAN_POINT('Origin',(11.8728378521018,-5.15773882741455,-1.));
#10879=CARTESIAN_POINT('',(9.34985040397592,-8.18776194312925,-0.999999999999996));
#10880=CARTESIAN_POINT('Origin',(9.55384714006266,-8.36463854323778,-0.999999999999996));
#10881=CARTESIAN_POINT('Origin',(1.0842021724855E-13,-0.0809177714881883,
-0.999999999999996));
#10882=CARTESIAN_POINT('Origin',(6.29005919429151,-11.3580426722999,-0.999999999999996));
#10883=CARTESIAN_POINT('',(7.82303414640502,-9.98886158592504,-0.999999999999996));
#10884=CARTESIAN_POINT('Origin',(10.557857409218,-7.51529989933299,-1.));
#10885=CARTESIAN_POINT('',(7.46002606094704,-9.95455115388547,-0.999999999999996));
#10886=CARTESIAN_POINT('Origin',(7.62279026591315,-10.1699758822287,-0.999999999999996));
#10887=CARTESIAN_POINT('Origin',(2.12937306676153E-13,-0.0809177714885291,
-0.999999999999996));
#10888=CARTESIAN_POINT('Origin',(3.80796020367903,-12.4193872788215,-0.999999999999996));
#10889=CARTESIAN_POINT('',(5.59210472977776,-11.3988494984891,-0.999999999999996));
#10890=CARTESIAN_POINT('Origin',(8.78144793533066,-9.54794279814123,-0.999999999999996));
#10891=CARTESIAN_POINT('',(5.2441627818781,-11.2898152068813,-0.999999999999996));
#10892=CARTESIAN_POINT('Origin',(5.35858087893726,-11.5343729691081,-0.999999999999996));
#10893=CARTESIAN_POINT('Origin',(-2.38004060904018E-12,-0.0809177714827325,
-0.999999999999996));
#10894=CARTESIAN_POINT('',(3.11677350256355,-12.3141894851212,-0.999999999999996));
#10895=CARTESIAN_POINT('Origin',(6.62124704860706,-11.1668312754584,-1.));
#10896=CARTESIAN_POINT('',(2.79910442495613,-12.1351966556931,-0.999999999999996));
#10897=CARTESIAN_POINT('Origin',(2.8601757942279,-12.3981991040758,-0.999999999999996));
#10898=CARTESIAN_POINT('Origin',(-5.72241906637849E-13,-0.0809177714854283,
-0.999999999999996));
#10899=CARTESIAN_POINT('',(1.16340283080872,-14.4338440882107,-0.999999999999996));
#10900=CARTESIAN_POINT('Origin',(9.19403442267708E-14,-0.0809177714883105,
-1.00000000000057));
#10901=CARTESIAN_POINT('',(0.505224317348871,-12.694876796117,-0.999999999999996));
#10902=CARTESIAN_POINT('Origin',(4.17166589359103,-12.3012121365371,-1.));
#10903=CARTESIAN_POINT('',(0.231711773070495,-12.4537482744175,-0.999999999999996));
#10904=CARTESIAN_POINT('Origin',(0.23676730266476,-12.723700939936,-0.999999999999996));
#10905=CARTESIAN_POINT('',(-0.231711773070466,-12.4537482744175,-0.999999999999996));
#10906=CARTESIAN_POINT('Origin',(1.27664805810168E-14,-0.0809177714956016,
-0.999999999999996));
#10907=CARTESIAN_POINT('',(-0.505224317348839,-12.694876796117,-0.999999999999996));
#10908=CARTESIAN_POINT('Origin',(-0.236767302664738,-12.723700939936,-0.999999999999996));
#10909=CARTESIAN_POINT('Origin',(-4.171665893591,-12.3012121365371,-0.999999999999996));
#10910=CARTESIAN_POINT('',(-2.12840559486936,-12.5242735692457,-0.999999999999996));
#10911=CARTESIAN_POINT('Origin',(1.53976292115102,-12.9015074943849,-0.999999999999996));
#10912=CARTESIAN_POINT('',(-2.34580779517493,-12.231547828736,-0.999999999999996));
#10913=CARTESIAN_POINT('Origin',(-2.39698905616056,-12.4966524845305,-0.999999999999996));
#10914=CARTESIAN_POINT('',(-2.79910442495626,-12.1351966556931,-0.999999999999996));
#10915=CARTESIAN_POINT('Origin',(6.0281640790194E-13,-0.0809177714853745,
-0.999999999999996));
#10916=CARTESIAN_POINT('',(-3.11677350256368,-12.3141894851212,-0.999999999999996));
#10917=CARTESIAN_POINT('Origin',(-2.86017579422803,-12.3981991040758,-0.999999999999996));
#10918=CARTESIAN_POINT('Origin',(-6.62124704860716,-11.1668312754584,-0.999999999999996));
#10919=CARTESIAN_POINT('',(-4.66901396936862,-11.8098359841665,-0.999999999999996));
#10920=CARTESIAN_POINT('Origin',(-1.15943507954551,-12.9414815613271,-1.));
#10921=CARTESIAN_POINT('',(-4.82080430633652,-11.4783065443609,-0.999999999999996));
#10922=CARTESIAN_POINT('Origin',(-4.92598549120204,-11.72697684486,-0.999999999999996));
#10923=CARTESIAN_POINT('',(-5.24416278187822,-11.2898152068813,-0.999999999999996));
#10924=CARTESIAN_POINT('Origin',(2.17707796235089E-13,-0.0809177714876878,
-0.999999999999996));
#10925=CARTESIAN_POINT('',(-5.59210472977788,-11.398849498489,-0.999999999999996));
#10926=CARTESIAN_POINT('Origin',(-5.35858087893738,-11.534372969108,-0.999999999999996));
#10927=CARTESIAN_POINT('Origin',(-8.78144793533077,-9.54794279814109,-0.999999999999996));
#10928=CARTESIAN_POINT('',(-7.00556402899171,-10.5827883915993,-0.999999999999996));
#10929=CARTESIAN_POINT('Origin',(-3.80796020367914,-12.4193872788215,-1.));
#10930=CARTESIAN_POINT('',(-7.0851085365256,-10.2269446798721,-0.999999999999996));
#10931=CARTESIAN_POINT('Origin',(-7.23969272277707,-10.4483125396914,-0.999999999999996));
#10932=CARTESIAN_POINT('',(-7.46002606094714,-9.95455115388536,-0.999999999999996));
#10933=CARTESIAN_POINT('Origin',(-1.9298798670242E-13,-0.0809177714885872,
-0.999999999999996));
#10934=CARTESIAN_POINT('',(-7.82303414640512,-9.98886158592494,-0.999999999999996));
#10935=CARTESIAN_POINT('Origin',(-7.62279026591326,-10.1699758822286,-0.999999999999996));
#10936=CARTESIAN_POINT('Origin',(-10.5578574092181,-7.51529989933288,-0.999999999999996));
#10937=CARTESIAN_POINT('',(-0.749999999999984,3.66908222851188,-0.999999999999996));
#10938=CARTESIAN_POINT('',(-0.749999999999984,3.66908222851188,-0.999999999999996));
#10939=CARTESIAN_POINT('',(0.750000000000016,3.66908222851188,-0.999999999999996));
#10940=CARTESIAN_POINT('',(0.750000000000016,3.66908222851188,-0.999999999999996));
#10941=CARTESIAN_POINT('',(-0.749999999999984,3.66908222851188,-0.999999999999996));
#10942=CARTESIAN_POINT('Origin',(1.61979340522206E-14,-0.0809177714881199,
1.));
#10943=CARTESIAN_POINT('',(-9.03593732412197,-8.89675865936698,1.));
#10944=CARTESIAN_POINT('Origin',(-6.29005919429161,-11.3580426722998,1.));
#10945=CARTESIAN_POINT('',(-7.82303414640512,-9.98886158592494,1.));
#10946=CARTESIAN_POINT('Origin',(-10.5578574092181,-7.51529989933286,1.00000000000001));
#10947=CARTESIAN_POINT('',(-7.46002606094714,-9.95455115388536,1.));
#10948=CARTESIAN_POINT('Origin',(-7.62279026591326,-10.1699758822286,1.));
#10949=CARTESIAN_POINT('',(-7.0851085365256,-10.2269446798721,1.));
#10950=CARTESIAN_POINT('Origin',(-1.9298798670242E-13,-0.0809177714885872,
1.));
#10951=CARTESIAN_POINT('',(-7.00556402899171,-10.5827883915993,1.));
#10952=CARTESIAN_POINT('Origin',(-7.23969272277707,-10.4483125396914,1.));
#10953=CARTESIAN_POINT('Origin',(-3.80796020367915,-12.4193872788215,1.));
#10954=CARTESIAN_POINT('',(-5.59210472977788,-11.398849498489,1.));
#10955=CARTESIAN_POINT('Origin',(-8.78144793533078,-9.54794279814109,1.));
#10956=CARTESIAN_POINT('',(-5.24416278187822,-11.2898152068813,1.));
#10957=CARTESIAN_POINT('Origin',(-5.35858087893738,-11.534372969108,1.));
#10958=CARTESIAN_POINT('',(-4.82080430633652,-11.4783065443609,1.));
#10959=CARTESIAN_POINT('Origin',(2.17707796235089E-13,-0.0809177714876878,
1.));
#10960=CARTESIAN_POINT('',(-4.66901396936862,-11.8098359841665,1.));
#10961=CARTESIAN_POINT('Origin',(-4.92598549120204,-11.72697684486,1.));
#10962=CARTESIAN_POINT('Origin',(-1.15943507954552,-12.9414815613271,1.00000000000001));
#10963=CARTESIAN_POINT('',(-3.11677350256368,-12.3141894851212,1.));
#10964=CARTESIAN_POINT('Origin',(-6.62124704860717,-11.1668312754584,1.00000000000001));
#10965=CARTESIAN_POINT('',(-2.79910442495626,-12.1351966556931,1.));
#10966=CARTESIAN_POINT('Origin',(-2.86017579422803,-12.3981991040758,1.));
#10967=CARTESIAN_POINT('',(-2.34580779517493,-12.231547828736,1.));
#10968=CARTESIAN_POINT('Origin',(6.0281640790194E-13,-0.0809177714853745,
1.));
#10969=CARTESIAN_POINT('',(-2.12840559486936,-12.5242735692457,1.));
#10970=CARTESIAN_POINT('Origin',(-2.39698905616056,-12.4966524845305,1.));
#10971=CARTESIAN_POINT('Origin',(1.53976292115103,-12.9015074943849,1.00000000000001));
#10972=CARTESIAN_POINT('',(-0.505224317348839,-12.694876796117,1.));
#10973=CARTESIAN_POINT('Origin',(-4.171665893591,-12.3012121365371,1.));
#10974=CARTESIAN_POINT('',(-0.231711773070466,-12.4537482744175,1.));
#10975=CARTESIAN_POINT('Origin',(-0.236767302664738,-12.723700939936,1.));
#10976=CARTESIAN_POINT('',(0.231711773070495,-12.4537482744175,1.));
#10977=CARTESIAN_POINT('Origin',(1.27664805810168E-14,-0.0809177714956016,
1.));
#10978=CARTESIAN_POINT('',(0.505224317348871,-12.694876796117,1.));
#10979=CARTESIAN_POINT('Origin',(0.23676730266476,-12.723700939936,1.));
#10980=CARTESIAN_POINT('',(1.16340283080871,-14.4338440882107,1.));
#10981=CARTESIAN_POINT('Origin',(4.17166589359103,-12.3012121365371,1.));
#10982=CARTESIAN_POINT('Origin',(4.2858511878352E-13,-0.0809177714923429,
1.00000000000058));
#10983=CARTESIAN_POINT('',(2.79910442495613,-12.1351966556931,1.));
#10984=CARTESIAN_POINT('Origin',(-5.72241906637849E-13,-0.0809177714854283,
1.));
#10985=CARTESIAN_POINT('',(3.11677350256355,-12.3141894851212,1.));
#10986=CARTESIAN_POINT('Origin',(2.8601757942279,-12.3981991040758,1.));
#10987=CARTESIAN_POINT('Origin',(6.62124704860705,-11.1668312754585,1.));
#10988=CARTESIAN_POINT('',(5.2441627818781,-11.2898152068813,1.));
#10989=CARTESIAN_POINT('Origin',(-2.38004060904018E-12,-0.0809177714827325,
1.));
#10990=CARTESIAN_POINT('',(5.59210472977776,-11.3988494984891,1.));
#10991=CARTESIAN_POINT('Origin',(5.35858087893726,-11.5343729691081,1.));
#10992=CARTESIAN_POINT('Origin',(8.78144793533065,-9.54794279814124,1.));
#10993=CARTESIAN_POINT('Origin',(3.80796020367901,-12.4193872788215,1.));
#10994=CARTESIAN_POINT('',(7.46002606094704,-9.95455115388547,1.));
#10995=CARTESIAN_POINT('Origin',(2.12937306676153E-13,-0.0809177714885291,
1.));
#10996=CARTESIAN_POINT('',(7.82303414640502,-9.98886158592504,1.));
#10997=CARTESIAN_POINT('Origin',(7.62279026591315,-10.1699758822287,1.));
#10998=CARTESIAN_POINT('Origin',(10.557857409218,-7.515299899333,1.00000000000001));
#10999=CARTESIAN_POINT('Origin',(6.29005919429151,-11.3580426722999,1.));
#11000=CARTESIAN_POINT('',(9.34985040397592,-8.18776194312925,1.));
#11001=CARTESIAN_POINT('Origin',(1.0842021724855E-13,-0.0809177714881883,
1.));
#11002=CARTESIAN_POINT('',(9.71205943175165,-8.14584898508081,1.));
#11003=CARTESIAN_POINT('Origin',(9.55384714006266,-8.36463854323778,1.));
#11004=CARTESIAN_POINT('Origin',(11.8728378521018,-5.15773882741455,1.));
#11005=CARTESIAN_POINT('Origin',(8.49725241506067,-9.80383359396364,1.));
#11006=CARTESIAN_POINT('',(10.8310414187911,-6.06666474111799,1.));
#11007=CARTESIAN_POINT('Origin',(2.35835656559047E-12,-0.0809177714894533,
1.));
#11008=CARTESIAN_POINT('',(11.176621116299,-5.95036019036894,1.));
#11009=CARTESIAN_POINT('Origin',(11.0673550497465,-6.197262856819,1.));
#11010=CARTESIAN_POINT('Origin',(12.6689183086518,-2.57829631406185,1.));
#11011=CARTESIAN_POINT('Origin',(10.3330749309508,-7.82468643845875,1.));
#11012=CARTESIAN_POINT('',(11.838863950502,-3.68396167373318,1.));
#11013=CARTESIAN_POINT('Origin',(-2.20223145275256E-12,-0.0809177714873727,
1.));
#11014=CARTESIAN_POINT('',(12.1527108266856,-3.49834859724242,1.));
#11015=CARTESIAN_POINT('Origin',(12.0971664366947,-3.76257354069125,1.));
#11016=CARTESIAN_POINT('Origin',(12.9113062428988,0.11029362535318,1.00000000000001));
#11017=CARTESIAN_POINT('Origin',(11.7172924887636,-5.50709943348251,1.00000000000001));
#11018=CARTESIAN_POINT('',(12.3292713184038,-1.14378829849741,1.));
#11019=CARTESIAN_POINT('Origin',(-5.25534477047174E-12,-0.08091777148747,
1.));
#11020=CARTESIAN_POINT('',(12.5976687587696,-0.896978878377931,1.));
#11021=CARTESIAN_POINT('Origin',(12.5982736017145,-1.16697820090489,1.));
#11022=CARTESIAN_POINT('Origin',(12.58940813901,2.79052670919212,1.));
#11023=CARTESIAN_POINT('',(12.5976687587696,0.735143335401439,1.));
#11024=CARTESIAN_POINT('Origin',(12.5894081390099,-2.95236225216863,1.00000000000001));
#11025=CARTESIAN_POINT('',(12.3292713184039,0.981952755520918,1.));
#11026=CARTESIAN_POINT('Origin',(12.5982736017145,1.00514265792839,1.));
#11027=CARTESIAN_POINT('Origin',(-1.40512601554121E-12,-0.0809177714882771,
1.));
#11028=CARTESIAN_POINT('Origin',(11.7172924887637,5.345263890506,1.));
#11029=CARTESIAN_POINT('',(12.1527108266857,3.33651305426593,1.));
#11030=CARTESIAN_POINT('Origin',(12.9113062428988,-0.272129168329664,1.00000000000001));
#11031=CARTESIAN_POINT('',(11.838863950502,3.5221261307567,1.));
#11032=CARTESIAN_POINT('Origin',(12.0971664366948,3.60073799771477,1.));
#11033=CARTESIAN_POINT('Origin',(1.47104550762833E-12,-0.0809177714876732,
1.));
#11034=CARTESIAN_POINT('Origin',(10.3330749309509,7.66285089548231,1.));
#11035=CARTESIAN_POINT('',(11.1766211162991,5.78852464739247,1.));
#11036=CARTESIAN_POINT('Origin',(12.6689183086518,2.41646077108532,1.00000000000001));
#11037=CARTESIAN_POINT('',(10.8310414187912,5.90482919814151,1.));
#11038=CARTESIAN_POINT('Origin',(11.0673550497466,6.03542731384252,1.));
#11039=CARTESIAN_POINT('Origin',(-4.47558656802016E-13,-0.0809177714884237,
1.));
#11040=CARTESIAN_POINT('Origin',(8.49725241506088,9.64199805098721,1.));
#11041=CARTESIAN_POINT('',(9.71205943175181,7.98401344210438,1.));
#11042=CARTESIAN_POINT('Origin',(11.8728378521019,4.99590328443805,1.00000000000001));
#11043=CARTESIAN_POINT('',(9.34985040397608,8.02592640015281,1.));
#11044=CARTESIAN_POINT('Origin',(9.55384714006283,8.20280300026134,1.));
#11045=CARTESIAN_POINT('Origin',(1.21430643318376E-14,-0.080917771488098,
1.));
#11046=CARTESIAN_POINT('Origin',(6.29005919429173,11.1962071293235,1.00000000000001));
#11047=CARTESIAN_POINT('',(7.82303414640522,9.82702604294864,1.));
#11048=CARTESIAN_POINT('Origin',(10.5578574092182,7.35346435635655,1.00000000000001));
#11049=CARTESIAN_POINT('',(7.46002606094724,9.79271561090908,1.));
#11050=CARTESIAN_POINT('Origin',(7.62279026591336,10.0081403392523,1.));
#11051=CARTESIAN_POINT('Origin',(-7.51135265097957E-13,-0.0809177714892022,
1.));
#11052=CARTESIAN_POINT('Origin',(3.80796020367927,12.2575517358452,1.));
#11053=CARTESIAN_POINT('',(5.59210472977799,11.2370139555127,1.));
#11054=CARTESIAN_POINT('Origin',(8.78144793533088,9.38610725516479,1.));
#11055=CARTESIAN_POINT('',(5.24416278187833,11.127979663905,1.));
#11056=CARTESIAN_POINT('Origin',(5.35858087893749,11.3725374261318,1.));
#11057=CARTESIAN_POINT('Origin',(-9.87925019568792E-13,-0.0809177714904624,
1.));
#11058=CARTESIAN_POINT('',(3.11677350256379,12.1523539421449,1.));
#11059=CARTESIAN_POINT('Origin',(6.62124704860725,11.0049957324821,1.));
#11060=CARTESIAN_POINT('',(2.79910442495637,11.9733611127168,1.));
#11061=CARTESIAN_POINT('Origin',(2.86017579422815,12.2363635610995,1.));
#11062=CARTESIAN_POINT('Origin',(9.63855731339613E-13,-0.0809177714833623,
1.));
#11063=CARTESIAN_POINT('',(0.505224317348871,12.5330412531408,1.));
#11064=CARTESIAN_POINT('Origin',(4.17166589359102,12.1393765935609,1.00000000000001));
#11065=CARTESIAN_POINT('',(0.231711773070499,12.2919127314413,1.));
#11066=CARTESIAN_POINT('Origin',(0.236767302664761,12.5618653969598,1.));
#11067=CARTESIAN_POINT('',(-0.231711773070462,12.2919127314413,1.));
#11068=CARTESIAN_POINT('Origin',(1.82145964977565E-14,-0.0809177714804904,
1.));
#11069=CARTESIAN_POINT('',(-0.505224317348839,12.5330412531408,1.));
#11070=CARTESIAN_POINT('Origin',(-0.236767302664724,12.5618653969598,1.));
#11071=CARTESIAN_POINT('Origin',(-4.17166589359098,12.1393765935609,1.));
#11072=CARTESIAN_POINT('',(-2.12840559486928,12.3624380262694,1.));
#11073=CARTESIAN_POINT('Origin',(1.53976292115111,12.7396719514087,1.));
#11074=CARTESIAN_POINT('',(-2.34580779517484,12.0697122857598,1.));
#11075=CARTESIAN_POINT('Origin',(-2.39698905616047,12.3348169415543,1.));
#11076=CARTESIAN_POINT('',(-2.79910442495618,11.9733611127169,1.));
#11077=CARTESIAN_POINT('Origin',(-1.83013326715553E-13,-0.0809177714870919,
1.));
#11078=CARTESIAN_POINT('',(-3.11677350256359,12.1523539421449,1.));
#11079=CARTESIAN_POINT('Origin',(-2.86017579422795,12.2363635610995,1.));
#11080=CARTESIAN_POINT('Origin',(-6.62124704860709,11.0049957324822,1.));
#11081=CARTESIAN_POINT('',(-4.66901396936854,11.6480004411903,1.));
#11082=CARTESIAN_POINT('Origin',(-1.15943507954541,12.7796460183509,1.00000000000001));
#11083=CARTESIAN_POINT('',(-4.82080430633644,11.3164710013847,1.));
#11084=CARTESIAN_POINT('Origin',(-4.92598549120196,11.5651413018838,1.));
#11085=CARTESIAN_POINT('',(-5.24416278187814,11.1279796639051,1.));
#11086=CARTESIAN_POINT('Origin',(-2.89265139619133E-13,-0.0809177714872558,
1.));
#11087=CARTESIAN_POINT('',(-5.5921047297778,11.2370139555128,1.));
#11088=CARTESIAN_POINT('Origin',(-5.3585808789373,11.3725374261318,1.));
#11089=CARTESIAN_POINT('Origin',(-8.78144793533071,9.38610725516491,1.));
#11090=CARTESIAN_POINT('',(-7.00556402899164,10.4209528486231,1.));
#11091=CARTESIAN_POINT('Origin',(-3.80796020367908,12.2575517358452,1.00000000000001));
#11092=CARTESIAN_POINT('',(-7.08510853652553,10.0651091368959,1.));
#11093=CARTESIAN_POINT('Origin',(-7.239692722777,10.2864769967152,1.));
#11094=CARTESIAN_POINT('',(-7.46002606094707,9.79271561090918,1.));
#11095=CARTESIAN_POINT('Origin',(4.36716635077161E-13,-0.080917771488739,
1.));
#11096=CARTESIAN_POINT('',(-7.82303414640506,9.82702604294875,1.));
#11097=CARTESIAN_POINT('Origin',(-7.62279026591319,10.0081403392524,1.));
#11098=CARTESIAN_POINT('Origin',(-10.557857409218,7.3534643563567,1.));
#11099=CARTESIAN_POINT('',(-9.03593732412191,8.7349231163908,1.));
#11100=CARTESIAN_POINT('Origin',(-6.29005919429155,11.1962071293236,1.00000000000001));
#11101=CARTESIAN_POINT('',(-9.03975952554566,8.37031721047198,1.));
#11102=CARTESIAN_POINT('Origin',(-9.23699064246666,8.55470779189656,1.));
#11103=CARTESIAN_POINT('',(-9.34985040397594,8.02592640015294,1.));
#11104=CARTESIAN_POINT('Origin',(-2.06258621293642E-12,-0.0809177714861846,
1.));
#11105=CARTESIAN_POINT('',(-9.71205943175167,7.98401344210451,1.));
#11106=CARTESIAN_POINT('Origin',(-9.55384714006268,8.20280300026148,1.));
#11107=CARTESIAN_POINT('Origin',(-11.8728378521018,4.99590328443823,1.));
#11108=CARTESIAN_POINT('',(-10.6713967989501,6.66359883426014,1.));
#11109=CARTESIAN_POINT('Origin',(-8.49725241506071,9.64199805098735,1.));
#11110=CARTESIAN_POINT('',(-10.5993296457206,6.30616576181161,1.));
#11111=CARTESIAN_POINT('Origin',(-10.8305877470818,6.44552031162906,1.));
#11112=CARTESIAN_POINT('',(-10.8310414187911,5.90482919814167,1.));
#11113=CARTESIAN_POINT('Origin',(-1.49966844498195E-12,-0.0809177714873426,
1.));
#11114=CARTESIAN_POINT('',(-11.176621116299,5.78852464739262,1.));
#11115=CARTESIAN_POINT('Origin',(-11.0673550497465,6.03542731384268,1.));
#11116=CARTESIAN_POINT('Origin',(-12.6689183086518,2.41646077108552,1.));
#11117=CARTESIAN_POINT('',(-11.8404650266211,4.29750681267689,1.));
#11118=CARTESIAN_POINT('Origin',(-10.3330749309508,7.66285089548245,1.));
#11119=CARTESIAN_POINT('',(-11.6956581991509,3.96286811411883,1.));
#11120=CARTESIAN_POINT('Origin',(-11.9508361962233,4.0510961698048,1.));
#11121=CARTESIAN_POINT('',(-11.838863950502,3.52212613075686,1.));
#11122=CARTESIAN_POINT('Origin',(4.26828711264093E-12,-0.080917771489527,
1.));
#11123=CARTESIAN_POINT('',(-12.1527108266856,3.3365130542661,1.));
#11124=CARTESIAN_POINT('Origin',(-12.0971664366947,3.60073799771494,1.));
#11125=CARTESIAN_POINT('Origin',(-12.9113062428988,-0.272129168329465,1.));
#11126=CARTESIAN_POINT('',(-12.4920481157737,1.74005662675346,1.));
#11127=CARTESIAN_POINT('Origin',(-11.7172924887636,5.3452638905062,1.00000000000001));
#11128=CARTESIAN_POINT('',(-12.2808303672836,1.44283761898748,1.));
#11129=CARTESIAN_POINT('Origin',(-12.5487757571153,1.47608319114332,1.));
#11130=CARTESIAN_POINT('',(-12.3292713184038,0.981952755521089,1.));
#11131=CARTESIAN_POINT('Origin',(-2.37310171513627E-12,-0.0809177714879208,
1.));
#11132=CARTESIAN_POINT('',(-12.5976687587696,0.735143335401609,1.));
#11133=CARTESIAN_POINT('Origin',(-12.5982736017144,1.00514265792856,1.));
#11134=CARTESIAN_POINT('Origin',(-12.5894081390099,-2.95236225216843,1.));
#11135=CARTESIAN_POINT('',(-12.5976687587696,-0.896978878377764,1.));
#11136=CARTESIAN_POINT('Origin',(-12.5894081390099,2.79052670919229,1.));
#11137=CARTESIAN_POINT('',(-12.3292713184038,-1.14378829849724,1.));
#11138=CARTESIAN_POINT('Origin',(-12.5982736017144,-1.16697820090472,1.));
#11139=CARTESIAN_POINT('',(-12.2808303672837,-1.60467316196364,1.));
#11140=CARTESIAN_POINT('Origin',(5.0558515707344E-12,-0.0809177714875954,
1.));
#11141=CARTESIAN_POINT('',(-12.4920481157737,-1.90189216972961,1.));
#11142=CARTESIAN_POINT('Origin',(-12.5487757571153,-1.63791873411946,1.));
#11143=CARTESIAN_POINT('Origin',(-11.7172924887636,-5.50709943348232,1.));
#11144=CARTESIAN_POINT('',(-12.1527108266856,-3.49834859724226,1.));
#11145=CARTESIAN_POINT('Origin',(-12.9113062428988,0.110293625353339,1.00000000000001));
#11146=CARTESIAN_POINT('',(-11.838863950502,-3.68396167373302,1.));
#11147=CARTESIAN_POINT('Origin',(-12.0971664366948,-3.76257354069109,1.));
#11148=CARTESIAN_POINT('',(-11.6956581991509,-4.12470365709499,1.));
#11149=CARTESIAN_POINT('Origin',(9.35449634420493E-12,-0.0809177714850636,
1.));
#11150=CARTESIAN_POINT('',(-11.8404650266211,-4.45934235565306,1.));
#11151=CARTESIAN_POINT('Origin',(-11.9508361962233,-4.21293171278095,1.));
#11152=CARTESIAN_POINT('Origin',(-10.3330749309508,-7.82468643845864,1.));
#11153=CARTESIAN_POINT('',(-11.176621116299,-5.95036019036879,1.));
#11154=CARTESIAN_POINT('Origin',(-12.6689183086518,-2.57829631406167,1.00000000000001));
#11155=CARTESIAN_POINT('',(-10.8310414187911,-6.06666474111783,1.));
#11156=CARTESIAN_POINT('Origin',(-11.0673550497465,-6.19726285681884,1.));
#11157=CARTESIAN_POINT('',(-10.5993296457206,-6.46800130478777,1.));
#11158=CARTESIAN_POINT('Origin',(1.26721549920106E-12,-0.0809177714874432,
1.));
#11159=CARTESIAN_POINT('',(-10.6713967989502,-6.82543437723631,1.));
#11160=CARTESIAN_POINT('Origin',(-10.8305877470818,-6.60735585460522,1.));
#11161=CARTESIAN_POINT('Origin',(-8.49725241506079,-9.80383359396352,1.));
#11162=CARTESIAN_POINT('',(-9.71205943175173,-8.14584898508068,1.));
#11163=CARTESIAN_POINT('Origin',(-11.8728378521018,-5.15773882741439,1.));
#11164=CARTESIAN_POINT('',(-9.349850403976,-8.18776194312912,1.));
#11165=CARTESIAN_POINT('Origin',(-9.55384714006274,-8.36463854323765,1.));
#11166=CARTESIAN_POINT('',(-9.03975952554573,-8.53215275344816,1.));
#11167=CARTESIAN_POINT('Origin',(-1.94202293135604E-12,-0.0809177714900912,
1.));
#11168=CARTESIAN_POINT('Origin',(-9.23699064246671,-8.71654333487274,1.));
#11169=CARTESIAN_POINT('',(-0.749999999999984,3.66908222851188,1.));
#11170=CARTESIAN_POINT('',(-0.749999999999984,3.66908222851188,1.));
#11171=CARTESIAN_POINT('',(0.750000000000016,3.66908222851188,1.));
#11172=CARTESIAN_POINT('',(-0.749999999999984,3.66908222851188,1.));
#11173=CARTESIAN_POINT('',(0.750000000000016,3.66908222851188,1.));
#11174=CARTESIAN_POINT('Origin',(1.56125112837913E-14,-0.080917771488119,
1.));
#11175=CARTESIAN_POINT('',(1.16340283080872,-14.4338440882107,4.11429224827654E-15));
#11176=CARTESIAN_POINT('Origin',(-4.17166589359099,-12.3012121365371,-0.999999999999996));
#11177=CARTESIAN_POINT('',(-0.505224317348839,-12.694876796117,-0.999999999999996));
#11178=CARTESIAN_POINT('Origin',(4.17166589359102,-12.3012121365371,-0.999999999999996));
#11179=CARTESIAN_POINT('',(0.50522431734887,-12.694876796117,-0.999999999999996));
#11180=CARTESIAN_POINT('Origin',(1.56125112837913E-14,-0.0809177714881191,
-0.999999999999996));
#11181=CARTESIAN_POINT('',(-0.231711773070466,-12.4537482744175,-0.999999999999996));
#11182=CARTESIAN_POINT('',(0.231711773070495,-12.4537482744175,-0.999999999999996));
#11183=CARTESIAN_POINT('Origin',(-0.236767302664731,-12.723700939936,-0.999999999999996));
#11184=CARTESIAN_POINT('Origin',(0.23676730266476,-12.723700939936,-0.999999999999996));
#11185=CARTESIAN_POINT('Origin',(1.53976292115102,-12.9015074943849,-0.999999999999996));
#11186=CARTESIAN_POINT('',(-2.12840559486936,-12.5242735692457,-0.999999999999996));
#11187=CARTESIAN_POINT('Origin',(-6.62124704860716,-11.1668312754584,-0.999999999999996));
#11188=CARTESIAN_POINT('',(-3.11677350256368,-12.3141894851212,-0.999999999999996));
#11189=CARTESIAN_POINT('Origin',(-2.86017579422803,-12.3981991040758,-0.999999999999996));
#11190=CARTESIAN_POINT('',(-2.79910442495626,-12.1351966556931,-0.999999999999996));
#11191=CARTESIAN_POINT('Origin',(1.56125112837913E-14,-0.0809177714881191,
-0.999999999999996));
#11192=CARTESIAN_POINT('',(-2.34580779517493,-12.231547828736,-0.999999999999996));
#11193=CARTESIAN_POINT('Origin',(-2.39698905616056,-12.4966524845305,-0.999999999999996));
#11194=CARTESIAN_POINT('Origin',(10.3330749309509,7.66285089548231,-0.999999999999996));
#11195=CARTESIAN_POINT('Origin',(12.9113062428988,-0.272129168329664,-0.999999999999996));
#11196=CARTESIAN_POINT('',(12.1527108266857,3.33651305426593,-0.999999999999996));
#11197=CARTESIAN_POINT('Origin',(12.0971664366948,3.60073799771476,-0.999999999999996));
#11198=CARTESIAN_POINT('',(11.838863950502,3.5221261307567,-0.999999999999996));
#11199=CARTESIAN_POINT('Origin',(1.56125112837913E-14,-0.0809177714881191,
-0.999999999999996));
#11200=CARTESIAN_POINT('Origin',(8.49725241506087,9.64199805098723,-0.999999999999996));
#11201=CARTESIAN_POINT('Origin',(12.6689183086518,2.41646077108535,-0.999999999999996));
#11202=CARTESIAN_POINT('',(11.1766211162991,5.78852464739247,-0.999999999999996));
#11203=CARTESIAN_POINT('Origin',(11.0673550497466,6.03542731384252,-0.999999999999996));
#11204=CARTESIAN_POINT('',(10.8310414187912,5.90482919814151,-0.999999999999996));
#11205=CARTESIAN_POINT('Origin',(1.56125112837913E-14,-0.0809177714881191,
-0.999999999999996));
#11206=CARTESIAN_POINT('Origin',(3.80796020367927,12.2575517358452,-0.999999999999996));
#11207=CARTESIAN_POINT('Origin',(10.5578574092182,7.35346435635656,-0.999999999999996));
#11208=CARTESIAN_POINT('',(7.82303414640522,9.82702604294864,-0.999999999999996));
#11209=CARTESIAN_POINT('Origin',(7.62279026591336,10.0081403392523,-0.999999999999996));
#11210=CARTESIAN_POINT('',(7.46002606094724,9.79271561090908,-0.999999999999996));
#11211=CARTESIAN_POINT('Origin',(1.56125112837913E-14,-0.0809177714881191,
-0.999999999999996));
#11212=CARTESIAN_POINT('Origin',(6.29005919429173,11.1962071293235,-0.999999999999996));
#11213=CARTESIAN_POINT('Origin',(11.8728378521019,4.99590328443808,-0.999999999999996));
#11214=CARTESIAN_POINT('',(9.71205943175181,7.98401344210438,-0.999999999999996));
#11215=CARTESIAN_POINT('Origin',(9.55384714006284,8.20280300026134,-0.999999999999996));
#11216=CARTESIAN_POINT('',(9.34985040397608,8.02592640015281,-0.999999999999996));
#11217=CARTESIAN_POINT('Origin',(1.56125112837913E-14,-0.0809177714881191,
-0.999999999999996));
#11218=CARTESIAN_POINT('Origin',(11.7172924887637,5.34526389050601,-0.999999999999996));
#11219=CARTESIAN_POINT('Origin',(12.5894081390099,-2.95236225216862,-0.999999999999996));
#11220=CARTESIAN_POINT('',(12.5976687587696,0.735143335401439,-0.999999999999996));
#11221=CARTESIAN_POINT('Origin',(12.5982736017145,1.00514265792839,-0.999999999999996));
#11222=CARTESIAN_POINT('',(12.3292713184039,0.981952755520918,-0.999999999999996));
#11223=CARTESIAN_POINT('Origin',(1.56125112837913E-14,-0.0809177714881191,
-0.999999999999996));
#11224=CARTESIAN_POINT('Origin',(12.58940813901,2.79052670919212,-0.999999999999996));
#11225=CARTESIAN_POINT('',(12.5976687587696,-0.896978878377932,-0.999999999999996));
#11226=CARTESIAN_POINT('Origin',(11.7172924887636,-5.50709943348249,-0.999999999999996));
#11227=CARTESIAN_POINT('Origin',(1.56125112837913E-14,-0.0809177714881191,
-0.999999999999996));
#11228=CARTESIAN_POINT('',(12.3292713184038,-1.14378829849741,-0.999999999999996));
#11229=CARTESIAN_POINT('Origin',(12.5982736017145,-1.16697820090488,-0.999999999999996));
#11230=CARTESIAN_POINT('Origin',(12.9113062428988,0.110293625353165,-0.999999999999996));
#11231=CARTESIAN_POINT('',(12.1527108266856,-3.49834859724242,-0.999999999999996));
#11232=CARTESIAN_POINT('Origin',(10.3330749309508,-7.82468643845875,-0.999999999999996));
#11233=CARTESIAN_POINT('Origin',(1.56125112837913E-14,-0.0809177714881191,
-0.999999999999996));
#11234=CARTESIAN_POINT('',(11.838863950502,-3.68396167373318,-0.999999999999996));
#11235=CARTESIAN_POINT('Origin',(12.0971664366947,-3.76257354069125,-0.999999999999996));
#11236=CARTESIAN_POINT('Origin',(12.6689183086518,-2.57829631406185,-0.999999999999996));
#11237=CARTESIAN_POINT('',(11.176621116299,-5.95036019036894,-0.999999999999996));
#11238=CARTESIAN_POINT('Origin',(8.49725241506067,-9.80383359396365,-0.999999999999996));
#11239=CARTESIAN_POINT('Origin',(1.56125112837913E-14,-0.0809177714881191,
-0.999999999999996));
#11240=CARTESIAN_POINT('',(10.8310414187911,-6.06666474111799,-0.999999999999996));
#11241=CARTESIAN_POINT('Origin',(11.0673550497465,-6.197262856819,-0.999999999999996));
#11242=CARTESIAN_POINT('Origin',(10.557857409218,-7.51529989933301,-0.999999999999996));
#11243=CARTESIAN_POINT('',(7.82303414640502,-9.98886158592504,-0.999999999999996));
#11244=CARTESIAN_POINT('Origin',(3.80796020367901,-12.4193872788215,-0.999999999999996));
#11245=CARTESIAN_POINT('Origin',(1.56125112837913E-14,-0.0809177714881191,
-0.999999999999996));
#11246=CARTESIAN_POINT('',(7.46002606094704,-9.95455115388547,-0.999999999999996));
#11247=CARTESIAN_POINT('Origin',(7.62279026591315,-10.1699758822287,-0.999999999999996));
#11248=CARTESIAN_POINT('Origin',(11.8728378521018,-5.15773882741456,-0.999999999999996));
#11249=CARTESIAN_POINT('',(9.71205943175165,-8.14584898508081,-0.999999999999996));
#11250=CARTESIAN_POINT('Origin',(6.2900591942915,-11.3580426722999,-0.999999999999996));
#11251=CARTESIAN_POINT('Origin',(1.56125112837913E-14,-0.0809177714881191,
-0.999999999999996));
#11252=CARTESIAN_POINT('',(9.34985040397592,-8.18776194312925,-0.999999999999996));
#11253=CARTESIAN_POINT('Origin',(9.55384714006266,-8.36463854323778,-0.999999999999996));
#11254=CARTESIAN_POINT('Origin',(8.78144793533068,-9.54794279814121,-0.999999999999996));
#11255=CARTESIAN_POINT('',(5.59210472977776,-11.3988494984891,-0.999999999999996));
#11256=CARTESIAN_POINT('Origin',(1.56125112837913E-14,-0.0809177714881191,
-0.999999999999996));
#11257=CARTESIAN_POINT('',(5.2441627818781,-11.2898152068813,-0.999999999999996));
#11258=CARTESIAN_POINT('Origin',(5.35858087893726,-11.5343729691081,-0.999999999999996));
#11259=CARTESIAN_POINT('Origin',(6.62124704860704,-11.1668312754585,-0.999999999999996));
#11260=CARTESIAN_POINT('',(3.11677350256355,-12.3141894851212,-0.999999999999996));
#11261=CARTESIAN_POINT('Origin',(1.56125112837913E-14,-0.0809177714881191,
-0.999999999999996));
#11262=CARTESIAN_POINT('',(2.79910442495613,-12.1351966556931,-0.999999999999996));
#11263=CARTESIAN_POINT('Origin',(2.8601757942279,-12.3981991040758,-0.999999999999996));
#11264=CARTESIAN_POINT('Origin',(8.78144793533087,9.3861072551648,-0.999999999999996));
#11265=CARTESIAN_POINT('',(5.59210472977799,11.2370139555127,-0.999999999999996));
#11266=CARTESIAN_POINT('Origin',(5.35858087893749,11.3725374261318,-0.999999999999996));
#11267=CARTESIAN_POINT('',(5.24416278187833,11.127979663905,-0.999999999999996));
#11268=CARTESIAN_POINT('Origin',(1.56125112837913E-14,-0.0809177714881191,
-0.999999999999996));
#11269=CARTESIAN_POINT('Origin',(6.62124704860727,11.0049957324821,-0.999999999999996));
#11270=CARTESIAN_POINT('',(3.11677350256379,12.1523539421449,-0.999999999999996));
#11271=CARTESIAN_POINT('Origin',(2.86017579422815,12.2363635610995,-0.999999999999996));
#11272=CARTESIAN_POINT('',(2.79910442495637,11.9733611127168,-0.999999999999996));
#11273=CARTESIAN_POINT('Origin',(1.56125112837913E-14,-0.0809177714881191,
-0.999999999999996));
#11274=CARTESIAN_POINT('Origin',(-4.17166589359099,12.1393765935609,-0.999999999999996));
#11275=CARTESIAN_POINT('',(-0.505224317348838,12.5330412531408,-0.999999999999996));
#11276=CARTESIAN_POINT('Origin',(4.17166589359102,12.1393765935609,-0.999999999999996));
#11277=CARTESIAN_POINT('',(0.505224317348871,12.5330412531408,-0.999999999999996));
#11278=CARTESIAN_POINT('Origin',(0.236767302664764,12.5618653969598,-0.999999999999996));
#11279=CARTESIAN_POINT('',(0.231711773070499,12.2919127314413,-0.999999999999996));
#11280=CARTESIAN_POINT('Origin',(1.56125112837913E-14,-0.0809177714881191,
-0.999999999999996));
#11281=CARTESIAN_POINT('',(-0.231711773070462,12.2919127314413,-0.999999999999996));
#11282=CARTESIAN_POINT('Origin',(-0.236767302664727,12.5618653969598,-0.999999999999996));
#11283=CARTESIAN_POINT('Origin',(-6.62124704860708,11.0049957324822,-0.999999999999996));
#11284=CARTESIAN_POINT('',(-3.11677350256359,12.1523539421449,-0.999999999999996));
#11285=CARTESIAN_POINT('Origin',(1.53976292115111,12.7396719514087,-0.999999999999996));
#11286=CARTESIAN_POINT('',(-2.12840559486928,12.3624380262694,-0.999999999999996));
#11287=CARTESIAN_POINT('Origin',(-2.39698905616047,12.3348169415543,-0.999999999999996));
#11288=CARTESIAN_POINT('',(-2.34580779517484,12.0697122857598,-0.999999999999996));
#11289=CARTESIAN_POINT('Origin',(1.56125112837913E-14,-0.0809177714881191,
-0.999999999999996));
#11290=CARTESIAN_POINT('',(-2.79910442495618,11.9733611127169,-0.999999999999996));
#11291=CARTESIAN_POINT('Origin',(-2.86017579422795,12.2363635610995,-0.999999999999996));
#11292=CARTESIAN_POINT('Origin',(-11.8728378521018,4.99590328443824,-0.999999999999996));
#11293=CARTESIAN_POINT('',(-9.71205943175167,7.98401344210451,-0.999999999999996));
#11294=CARTESIAN_POINT('Origin',(-6.29005919429154,11.1962071293236,-0.999999999999996));
#11295=CARTESIAN_POINT('',(-9.03593732412191,8.7349231163908,-0.999999999999996));
#11296=CARTESIAN_POINT('Origin',(-9.23699064246666,8.55470779189656,-0.999999999999996));
#11297=CARTESIAN_POINT('',(-9.03975952554566,8.37031721047198,-0.999999999999996));
#11298=CARTESIAN_POINT('Origin',(1.56125112837913E-14,-0.0809177714881191,
-0.999999999999996));
#11299=CARTESIAN_POINT('',(-9.34985040397594,8.02592640015294,-0.999999999999996));
#11300=CARTESIAN_POINT('Origin',(-9.55384714006268,8.20280300026147,-0.999999999999996));
#11301=CARTESIAN_POINT('Origin',(-12.6689183086518,2.41646077108552,-0.999999999999996));
#11302=CARTESIAN_POINT('',(-11.176621116299,5.78852464739263,-0.999999999999996));
#11303=CARTESIAN_POINT('Origin',(-8.49725241506071,9.64199805098735,-0.999999999999996));
#11304=CARTESIAN_POINT('',(-10.6713967989501,6.66359883426014,-0.999999999999996));
#11305=CARTESIAN_POINT('Origin',(-10.8305877470818,6.44552031162906,-0.999999999999996));
#11306=CARTESIAN_POINT('',(-10.5993296457206,6.30616576181161,-0.999999999999996));
#11307=CARTESIAN_POINT('Origin',(1.56125112837913E-14,-0.0809177714881191,
-0.999999999999996));
#11308=CARTESIAN_POINT('',(-10.8310414187911,5.90482919814167,-0.999999999999996));
#11309=CARTESIAN_POINT('Origin',(-11.0673550497465,6.03542731384268,-0.999999999999996));
#11310=CARTESIAN_POINT('Origin',(-10.557857409218,7.3534643563567,-0.999999999999996));
#11311=CARTESIAN_POINT('',(-7.82303414640506,9.82702604294875,-0.999999999999996));
#11312=CARTESIAN_POINT('Origin',(-3.80796020367907,12.2575517358453,-0.999999999999996));
#11313=CARTESIAN_POINT('',(-7.00556402899164,10.4209528486231,-0.999999999999996));
#11314=CARTESIAN_POINT('Origin',(-7.239692722777,10.2864769967152,-0.999999999999996));
#11315=CARTESIAN_POINT('',(-7.08510853652553,10.0651091368959,-0.999999999999996));
#11316=CARTESIAN_POINT('Origin',(1.56125112837913E-14,-0.0809177714881191,
-0.999999999999996));
#11317=CARTESIAN_POINT('',(-7.46002606094707,9.79271561090918,-0.999999999999996));
#11318=CARTESIAN_POINT('Origin',(-7.62279026591319,10.0081403392524,-0.999999999999996));
#11319=CARTESIAN_POINT('Origin',(-8.78144793533071,9.38610725516492,-0.999999999999996));
#11320=CARTESIAN_POINT('',(-5.5921047297778,11.2370139555128,-0.999999999999996));
#11321=CARTESIAN_POINT('Origin',(-1.15943507954543,12.7796460183509,-0.999999999999996));
#11322=CARTESIAN_POINT('',(-4.66901396936854,11.6480004411903,-0.999999999999996));
#11323=CARTESIAN_POINT('Origin',(-4.92598549120196,11.5651413018838,-0.999999999999996));
#11324=CARTESIAN_POINT('',(-4.82080430633644,11.3164710013847,-0.999999999999996));
#11325=CARTESIAN_POINT('Origin',(1.56125112837913E-14,-0.0809177714881191,
-0.999999999999996));
#11326=CARTESIAN_POINT('',(-5.24416278187814,11.1279796639051,-0.999999999999996));
#11327=CARTESIAN_POINT('Origin',(-5.3585808789373,11.3725374261318,-0.999999999999996));
#11328=CARTESIAN_POINT('Origin',(-12.9113062428988,-0.272129168329486,-0.999999999999996));
#11329=CARTESIAN_POINT('',(-12.1527108266856,3.3365130542661,-0.999999999999996));
#11330=CARTESIAN_POINT('Origin',(-10.3330749309508,7.66285089548245,-0.999999999999996));
#11331=CARTESIAN_POINT('',(-11.8404650266211,4.29750681267689,-0.999999999999996));
#11332=CARTESIAN_POINT('Origin',(-11.9508361962233,4.0510961698048,-0.999999999999996));
#11333=CARTESIAN_POINT('',(-11.6956581991509,3.96286811411883,-0.999999999999996));
#11334=CARTESIAN_POINT('Origin',(1.56125112837913E-14,-0.0809177714881191,
-0.999999999999996));
#11335=CARTESIAN_POINT('',(-11.838863950502,3.52212613075686,-0.999999999999996));
#11336=CARTESIAN_POINT('Origin',(-12.0971664366947,3.60073799771494,-0.999999999999996));
#11337=CARTESIAN_POINT('Origin',(-12.5894081390099,-2.95236225216845,-0.999999999999996));
#11338=CARTESIAN_POINT('',(-12.5976687587696,0.73514333540161,-0.999999999999996));
#11339=CARTESIAN_POINT('Origin',(-11.7172924887636,5.34526389050617,-0.999999999999996));
#11340=CARTESIAN_POINT('',(-12.4920481157737,1.74005662675346,-0.999999999999996));
#11341=CARTESIAN_POINT('Origin',(-12.5487757571153,1.47608319114332,-0.999999999999996));
#11342=CARTESIAN_POINT('',(-12.2808303672836,1.44283761898748,-0.999999999999996));
#11343=CARTESIAN_POINT('Origin',(1.56125112837913E-14,-0.0809177714881191,
-0.999999999999996));
#11344=CARTESIAN_POINT('',(-12.3292713184038,0.981952755521089,-0.999999999999996));
#11345=CARTESIAN_POINT('Origin',(-12.5982736017144,1.00514265792856,-0.999999999999996));
#11346=CARTESIAN_POINT('Origin',(-11.7172924887636,-5.50709943348233,-0.999999999999996));
#11347=CARTESIAN_POINT('',(-12.4920481157737,-1.90189216972961,-0.999999999999996));
#11348=CARTESIAN_POINT('Origin',(-12.5894081390099,2.79052670919229,-0.999999999999996));
#11349=CARTESIAN_POINT('',(-12.5976687587696,-0.896978878377764,-0.999999999999996));
#11350=CARTESIAN_POINT('Origin',(-12.5982736017144,-1.16697820090471,-0.999999999999996));
#11351=CARTESIAN_POINT('',(-12.3292713184038,-1.14378829849724,-0.999999999999996));
#11352=CARTESIAN_POINT('Origin',(1.56125112837913E-14,-0.0809177714881191,
-0.999999999999996));
#11353=CARTESIAN_POINT('',(-12.2808303672837,-1.60467316196364,-0.999999999999996));
#11354=CARTESIAN_POINT('Origin',(-12.5487757571153,-1.63791873411947,-0.999999999999996));
#11355=CARTESIAN_POINT('Origin',(-10.3330749309508,-7.82468643845862,-0.999999999999996));
#11356=CARTESIAN_POINT('',(-11.8404650266211,-4.45934235565305,-0.999999999999996));
#11357=CARTESIAN_POINT('Origin',(-12.9113062428988,0.110293625353334,-0.999999999999996));
#11358=CARTESIAN_POINT('',(-12.1527108266856,-3.49834859724226,-0.999999999999996));
#11359=CARTESIAN_POINT('Origin',(-12.0971664366948,-3.76257354069109,-0.999999999999996));
#11360=CARTESIAN_POINT('',(-11.838863950502,-3.68396167373302,-0.999999999999996));
#11361=CARTESIAN_POINT('Origin',(1.56125112837913E-14,-0.0809177714881191,
-0.999999999999996));
#11362=CARTESIAN_POINT('',(-11.6956581991509,-4.12470365709499,-0.999999999999996));
#11363=CARTESIAN_POINT('Origin',(-11.9508361962233,-4.21293171278096,-0.999999999999996));
#11364=CARTESIAN_POINT('Origin',(-1.15943507954552,-12.9414815613271,-0.999999999999996));
#11365=CARTESIAN_POINT('',(-4.66901396936862,-11.8098359841665,-0.999999999999996));
#11366=CARTESIAN_POINT('Origin',(-8.78144793533077,-9.5479427981411,-0.999999999999996));
#11367=CARTESIAN_POINT('',(-5.59210472977788,-11.398849498489,-0.999999999999996));
#11368=CARTESIAN_POINT('Origin',(-5.35858087893738,-11.534372969108,-0.999999999999996));
#11369=CARTESIAN_POINT('',(-5.24416278187822,-11.2898152068813,-0.999999999999996));
#11370=CARTESIAN_POINT('Origin',(1.56125112837913E-14,-0.0809177714881191,
-0.999999999999996));
#11371=CARTESIAN_POINT('',(-4.82080430633652,-11.4783065443609,-0.999999999999996));
#11372=CARTESIAN_POINT('Origin',(-4.92598549120204,-11.72697684486,-0.999999999999996));
#11373=CARTESIAN_POINT('Origin',(-3.80796020367915,-12.4193872788215,-0.999999999999996));
#11374=CARTESIAN_POINT('',(-7.00556402899171,-10.5827883915993,-0.999999999999996));
#11375=CARTESIAN_POINT('Origin',(-10.5578574092181,-7.51529989933287,-0.999999999999996));
#11376=CARTESIAN_POINT('',(-7.82303414640512,-9.98886158592494,-0.999999999999996));
#11377=CARTESIAN_POINT('Origin',(-7.62279026591326,-10.1699758822286,-0.999999999999996));
#11378=CARTESIAN_POINT('',(-7.46002606094714,-9.95455115388536,-0.999999999999996));
#11379=CARTESIAN_POINT('Origin',(1.56125112837913E-14,-0.0809177714881191,
-0.999999999999996));
#11380=CARTESIAN_POINT('',(-7.0851085365256,-10.2269446798721,-0.999999999999996));
#11381=CARTESIAN_POINT('Origin',(-7.23969272277707,-10.4483125396914,-0.999999999999996));
#11382=CARTESIAN_POINT('Origin',(-8.49725241506077,-9.80383359396353,-0.999999999999996));
#11383=CARTESIAN_POINT('',(-10.6713967989502,-6.82543437723631,-0.999999999999996));
#11384=CARTESIAN_POINT('Origin',(-12.6689183086518,-2.57829631406167,-0.999999999999996));
#11385=CARTESIAN_POINT('',(-11.176621116299,-5.95036019036879,-0.999999999999996));
#11386=CARTESIAN_POINT('Origin',(-11.0673550497465,-6.19726285681884,-0.999999999999996));
#11387=CARTESIAN_POINT('',(-10.8310414187911,-6.06666474111783,-0.999999999999996));
#11388=CARTESIAN_POINT('Origin',(1.56125112837913E-14,-0.0809177714881191,
-0.999999999999996));
#11389=CARTESIAN_POINT('',(-10.5993296457206,-6.46800130478777,-0.999999999999996));
#11390=CARTESIAN_POINT('Origin',(-10.8305877470818,-6.60735585460522,-0.999999999999996));
#11391=CARTESIAN_POINT('Origin',(-6.29005919429162,-11.3580426722998,-0.999999999999996));
#11392=CARTESIAN_POINT('',(-9.03593732412197,-8.89675865936698,-0.999999999999996));
#11393=CARTESIAN_POINT('Origin',(-11.8728378521018,-5.1577388274144,-0.999999999999996));
#11394=CARTESIAN_POINT('',(-9.71205943175173,-8.14584898508068,-0.999999999999996));
#11395=CARTESIAN_POINT('Origin',(-9.55384714006274,-8.36463854323765,-0.999999999999996));
#11396=CARTESIAN_POINT('',(-9.349850403976,-8.18776194312912,-0.999999999999996));
#11397=CARTESIAN_POINT('Origin',(1.56125112837913E-14,-0.0809177714881191,
-0.999999999999996));
#11398=CARTESIAN_POINT('',(-9.03975952554573,-8.53215275344816,-0.999999999999996));
#11399=CARTESIAN_POINT('Origin',(-9.23699064246672,-8.71654333487274,-0.999999999999996));
#11400=CARTESIAN_POINT('Origin',(-0.749999999999984,3.66908222851188,-0.999999999999996));
#11401=CARTESIAN_POINT('',(-0.749999999999984,3.66908222851188,-0.999999999999996));
#11402=CARTESIAN_POINT('Origin',(-0.749999999999984,3.66908222851188,-0.999999999999996));
#11403=CARTESIAN_POINT('',(0.750000000000016,3.66908222851188,-0.999999999999996));
#11404=CARTESIAN_POINT('Origin',(0.750000000000016,3.66908222851188,-0.999999999999996));
#11405=CARTESIAN_POINT('',(0.,0.,0.));
#11406=CARTESIAN_POINT('Origin',(22.,0.,3.));
#11407=CARTESIAN_POINT('',(23.5,-1.83697019872103E-16,4.));
#11408=CARTESIAN_POINT('Origin',(22.,0.,4.));
#11409=CARTESIAN_POINT('',(23.5,-1.83697019872103E-16,-1.));
#11410=CARTESIAN_POINT('',(23.5,-1.83697019872103E-16,3.));
#11411=CARTESIAN_POINT('Origin',(22.,0.,-1.));
#11412=CARTESIAN_POINT('Origin',(0.,0.,3.));
#11413=CARTESIAN_POINT('',(3.88651482573507,3.14563229086642,4.));
#11414=CARTESIAN_POINT('',(0.,-5.,4.));
#11415=CARTESIAN_POINT('Origin',(0.,0.,4.));
#11416=CARTESIAN_POINT('',(3.88651482573507,3.14563229086642,3.));
#11417=CARTESIAN_POINT('',(3.88651482573507,3.14563229086642,4.));
#11418=CARTESIAN_POINT('',(0.,5.,3.));
#11419=CARTESIAN_POINT('Origin',(0.,0.,3.));
#11420=CARTESIAN_POINT('',(0.,5.,0.));
#11421=CARTESIAN_POINT('',(0.,5.,3.));
#11422=CARTESIAN_POINT('',(3.88651482573507,3.14563229086642,0.));
#11423=CARTESIAN_POINT('Origin',(0.,0.,0.));
#11424=CARTESIAN_POINT('',(3.88651482573507,3.14563229086642,-1.));
#11425=CARTESIAN_POINT('',(3.88651482573507,3.14563229086642,-1.));
#11426=CARTESIAN_POINT('',(0.,-5.,-1.));
#11427=CARTESIAN_POINT('Origin',(0.,0.,-1.));
#11428=CARTESIAN_POINT('',(0.,-5.,3.));
#11429=CARTESIAN_POINT('Origin',(0.,0.,3.));
#11430=CARTESIAN_POINT('',(1.5,-1.83697019872103E-16,4.));
#11431=CARTESIAN_POINT('Origin',(0.,0.,4.));
#11432=CARTESIAN_POINT('',(1.5,-1.83697019872103E-16,-1.));
#11433=CARTESIAN_POINT('',(1.5,-1.83697019872103E-16,3.));
#11434=CARTESIAN_POINT('Origin',(0.,0.,-1.));
#11435=CARTESIAN_POINT('Origin',(0.,0.,4.));
#11436=CARTESIAN_POINT('',(45.2263053278443,6.62991522408338,4.));
#11437=CARTESIAN_POINT('',(45.4365685536382,6.10949547816422,4.));
#11438=CARTESIAN_POINT('',(45.2263053278443,6.62991522408338,4.));
#11439=CARTESIAN_POINT('',(54.708407099306,9.8555614123234,4.));
#11440=CARTESIAN_POINT('',(4.25411211450139,-10.5292969675612,4.));
#11441=CARTESIAN_POINT('',(52.2734642421026,15.8822564670075,4.));
#11442=CARTESIAN_POINT('',(55.4576202861379,8.00119370318982,4.));
#11443=CARTESIAN_POINT('',(20.7492131868318,3.14563229086643,4.));
#11444=CARTESIAN_POINT('',(20.7492131868318,3.14563229086643,4.));
#11445=CARTESIAN_POINT('',(22.7492131868318,3.14563229086642,4.));
#11446=CARTESIAN_POINT('',(22.,-5.,4.));
#11447=CARTESIAN_POINT('',(0.,-5.,4.));
#11448=CARTESIAN_POINT('',(26.8954874748715,-1.01695741473107,4.));
#11449=CARTESIAN_POINT('Origin',(22.,0.,4.));
#11450=CARTESIAN_POINT('',(29.9179419826634,2.60200444337179,4.));
#11451=CARTESIAN_POINT('Origin',(31.7909749497429,-2.03391482946214,4.));
#11452=CARTESIAN_POINT('',(42.622724431879,7.73506974638514,4.));
#11453=CARTESIAN_POINT('',(26.8147918762154,1.34825041766364,4.));
#11454=CARTESIAN_POINT('',(42.622724431879,7.73506974638514,4.));
#11455=CARTESIAN_POINT('Origin',(0.,0.,3.));
#11456=CARTESIAN_POINT('',(20.7492131868318,3.14563229086643,3.));
#11457=CARTESIAN_POINT('',(22.7492131868318,3.14563229086642,3.));
#11458=CARTESIAN_POINT('',(52.2734642421026,15.8822564670075,3.));
#11459=CARTESIAN_POINT('',(1.81916925729784,-4.50260191287694,3.));
#11460=CARTESIAN_POINT('',(51.5242510552708,17.7366241761411,3.));
#11461=CARTESIAN_POINT('',(50.4542949848047,20.3848583798845,3.));
#11462=CARTESIAN_POINT('',(20.,5.,3.));
#11463=CARTESIAN_POINT('',(1.06995607046601,-2.64823420374337,3.));
#11464=CARTESIAN_POINT('',(0.,5.,3.));
#11465=CARTESIAN_POINT('Origin',(0.,0.,-1.));
#11466=CARTESIAN_POINT('',(45.4365685536382,6.10949547816423,-1.));
#11467=CARTESIAN_POINT('',(54.708407099306,9.8555614123234,-1.));
#11468=CARTESIAN_POINT('',(4.25411211450139,-10.5292969675612,-1.));
#11469=CARTESIAN_POINT('',(45.2263053278443,6.62991522408338,-1.));
#11470=CARTESIAN_POINT('',(45.2263053278443,6.62991522408338,-1.));
#11471=CARTESIAN_POINT('',(42.622724431879,7.73506974638514,-1.));
#11472=CARTESIAN_POINT('',(42.622724431879,7.73506974638514,-1.));
#11473=CARTESIAN_POINT('',(29.9179419826634,2.60200444337179,-1.));
#11474=CARTESIAN_POINT('',(26.8147918762154,1.34825041766364,-1.));
#11475=CARTESIAN_POINT('',(26.8954874748715,-1.01695741473107,-1.));
#11476=CARTESIAN_POINT('Origin',(31.7909749497429,-2.03391482946214,-1.));
#11477=CARTESIAN_POINT('',(22.,-5.,-1.));
#11478=CARTESIAN_POINT('Origin',(22.,0.,-1.));
#11479=CARTESIAN_POINT('',(0.,-5.,-1.));
#11480=CARTESIAN_POINT('',(20.7492131868318,3.14563229086643,-1.));
#11481=CARTESIAN_POINT('',(22.7492131868318,3.14563229086642,-1.));
#11482=CARTESIAN_POINT('',(52.2734642421026,15.8822564670075,-1.));
#11483=CARTESIAN_POINT('',(20.7492131868318,3.14563229086643,-1.));
#11484=CARTESIAN_POINT('',(55.4576202861379,8.00119370318982,-1.));
#11485=CARTESIAN_POINT('Origin',(0.,0.,0.));
#11486=CARTESIAN_POINT('',(52.2734642421026,15.8822564670075,0.));
#11487=CARTESIAN_POINT('',(20.7492131868318,3.14563229086643,0.));
#11488=CARTESIAN_POINT('',(1.81916925729784,-4.50260191287694,0.));
#11489=CARTESIAN_POINT('',(22.7492131868318,3.14563229086642,0.));
#11490=CARTESIAN_POINT('',(20.,5.,0.));
#11491=CARTESIAN_POINT('',(0.,5.,0.));
#11492=CARTESIAN_POINT('',(51.5242510552708,17.7366241761411,0.));
#11493=CARTESIAN_POINT('',(1.06995607046601,-2.64823420374337,0.));
#11494=CARTESIAN_POINT('',(50.4542949848047,20.3848583798845,0.));
#11495=CARTESIAN_POINT('Origin',(22.7492131868318,3.14563229086642,4.));
#11496=CARTESIAN_POINT('',(20.7492131868318,3.14563229086643,4.));
#11497=CARTESIAN_POINT('Origin',(22.7492131868318,3.14563229086642,-1.));
#11498=CARTESIAN_POINT('',(20.7492131868318,3.14563229086643,-1.));
#11499=CARTESIAN_POINT('Origin',(0.,-5.,3.));
#11500=CARTESIAN_POINT('',(22.,-5.,3.));
#11501=CARTESIAN_POINT('Origin',(0.,5.,3.));
#11502=CARTESIAN_POINT('',(20.,5.,4.));
#11503=CARTESIAN_POINT('Origin',(22.,0.,3.));
#11504=CARTESIAN_POINT('',(26.8954874748715,-1.01695741473107,3.));
#11505=CARTESIAN_POINT('Origin',(3.29463570187568,-8.15450951250839,3.));
#11506=CARTESIAN_POINT('',(29.9179419826634,2.60200444337179,3.));
#11507=CARTESIAN_POINT('',(42.622724431879,7.73506974638514,3.));
#11508=CARTESIAN_POINT('Origin',(9.28931783023872,21.8842613872565,3.));
#11509=CARTESIAN_POINT('',(45.2263053278443,6.62991522408338,3.));
#11510=CARTESIAN_POINT('Origin',(41.1824564391369,16.6387924457253,3.));
#11511=CARTESIAN_POINT('',(45.4365685536382,6.10949547816422,-3.));
#11512=CARTESIAN_POINT('',(45.4365685536382,6.10949547816422,-3.));
#11513=CARTESIAN_POINT('',(46.18578174047,4.25512776903065,-3.));
#11514=CARTESIAN_POINT('',(41.1824564391368,16.6387924457254,-3.));
#11515=CARTESIAN_POINT('',(46.18578174047,4.25512776903065,6.));
#11516=CARTESIAN_POINT('',(46.18578174047,4.25512776903065,3.));
#11517=CARTESIAN_POINT('',(45.4365685536382,6.10949547816422,6.));
#11518=CARTESIAN_POINT('',(41.1824564391368,16.6387924457254,6.));
#11519=CARTESIAN_POINT('',(45.4365685536382,6.10949547816422,6.));
#11520=CARTESIAN_POINT('Origin',(5.00332530133316,-12.3836646766947,3.));
#11521=CARTESIAN_POINT('',(55.4576202861379,8.00119370318982,-3.));
#11522=CARTESIAN_POINT('',(5.00332530133317,-12.3836646766947,-3.));
#11523=CARTESIAN_POINT('',(55.4576202861379,8.00119370318982,6.));
#11524=CARTESIAN_POINT('',(55.4576202861379,8.00119370318982,3.));
#11525=CARTESIAN_POINT('',(5.00332530133317,-12.3836646766947,6.));
#11526=CARTESIAN_POINT('Origin',(50.4542949848047,20.3848583798845,3.));
#11527=CARTESIAN_POINT('',(52.2734642421026,15.8822564670075,4.));
#11528=CARTESIAN_POINT('',(54.708407099306,9.8555614123234,6.));
#11529=CARTESIAN_POINT('',(54.708407099306,9.8555614123234,6.));
#11530=CARTESIAN_POINT('',(50.4542949848046,20.3848583798846,6.));
#11531=CARTESIAN_POINT('',(54.708407099306,9.8555614123234,-3.));
#11532=CARTESIAN_POINT('',(50.4542949848046,20.3848583798846,-3.));
#11533=CARTESIAN_POINT('',(54.708407099306,9.8555614123234,-3.));
#11534=CARTESIAN_POINT('',(52.2734642421026,15.8822564670075,-1.));
#11535=CARTESIAN_POINT('',(51.5242510552708,17.7366241761411,3.));
#11536=CARTESIAN_POINT('Origin',(1.06995607046601,-2.64823420374337,3.));
#11537=CARTESIAN_POINT('Origin',(20.7492131868318,3.14563229086643,4.));
#11538=CARTESIAN_POINT('Origin',(20.7492131868318,3.14563229086643,-1.));
#11539=CARTESIAN_POINT('Origin',(4.25411211450139,-10.5292969675612,6.));
#11540=CARTESIAN_POINT('',(4.25411211450139,-10.5292969675612,6.));
#11541=CARTESIAN_POINT('Origin',(0.,0.,6.));
#11542=CARTESIAN_POINT('Origin',(4.25411211450139,-10.5292969675612,-3.));
#11543=CARTESIAN_POINT('',(4.25411211450139,-10.5292969675612,-3.));
#11544=CARTESIAN_POINT('Origin',(0.,0.,-3.));
#11545=CARTESIAN_POINT('Origin',(31.7909749497429,-2.03391482946214,3.));
#11546=CARTESIAN_POINT('',(0.,0.,0.));
#11547=CARTESIAN_POINT('Origin',(0.,0.,16.));
#11548=CARTESIAN_POINT('',(1.25,-1.53080849893419E-16,15.));
#11549=CARTESIAN_POINT('Origin',(0.,0.,15.));
#11550=CARTESIAN_POINT('',(1.25,-1.53080849893419E-16,16.));
#11551=CARTESIAN_POINT('',(1.25,-1.53080849893419E-16,16.));
#11552=CARTESIAN_POINT('',(-1.1842719282327,-0.4,16.));
#11553=CARTESIAN_POINT('Origin',(0.,0.,16.));
#11554=CARTESIAN_POINT('',(-1.1842719282327,-0.4,17.));
#11555=CARTESIAN_POINT('',(-1.1842719282327,-0.4,16.));
#11556=CARTESIAN_POINT('',(-1.1842719282327,0.4,17.));
#11557=CARTESIAN_POINT('Origin',(0.,0.,17.));
#11558=CARTESIAN_POINT('',(-1.1842719282327,0.4,16.));
#11559=CARTESIAN_POINT('',(-1.1842719282327,0.4,16.));
#11560=CARTESIAN_POINT('',(-0.4,1.1842719282327,16.));
#11561=CARTESIAN_POINT('Origin',(0.,0.,16.));
#11562=CARTESIAN_POINT('',(-0.4,1.1842719282327,17.));
#11563=CARTESIAN_POINT('',(-0.4,1.1842719282327,16.));
#11564=CARTESIAN_POINT('',(0.4,1.1842719282327,17.));
#11565=CARTESIAN_POINT('Origin',(0.,0.,17.));
#11566=CARTESIAN_POINT('',(0.4,1.1842719282327,16.));
#11567=CARTESIAN_POINT('',(0.4,1.1842719282327,16.));
#11568=CARTESIAN_POINT('Origin',(0.,0.,16.));
#11569=CARTESIAN_POINT('Origin',(0.,0.,15.));
#11570=CARTESIAN_POINT('',(1.5,-1.83697019872103E-16,2.));
#11571=CARTESIAN_POINT('Origin',(0.,0.,2.));
#11572=CARTESIAN_POINT('',(1.5,-1.83697019872103E-16,15.));
#11573=CARTESIAN_POINT('',(1.5,-1.83697019872103E-16,15.));
#11574=CARTESIAN_POINT('Origin',(0.,0.,15.));
#11575=CARTESIAN_POINT('Origin',(0.,0.,16.));
#11576=CARTESIAN_POINT('',(-1.4456832294801,0.4,16.));
#11577=CARTESIAN_POINT('',(-1.1842719282327,0.4,16.));
#11578=CARTESIAN_POINT('',(-0.4,1.4456832294801,16.));
#11579=CARTESIAN_POINT('Origin',(0.,0.,16.));
#11580=CARTESIAN_POINT('',(-0.4,1.1842719282327,16.));
#11581=CARTESIAN_POINT('Origin',(0.,0.,17.));
#11582=CARTESIAN_POINT('',(-1.4456832294801,0.4,17.));
#11583=CARTESIAN_POINT('',(-1.4456832294801,0.4,16.));
#11584=CARTESIAN_POINT('',(-0.4,1.4456832294801,17.));
#11585=CARTESIAN_POINT('Origin',(0.,0.,17.));
#11586=CARTESIAN_POINT('',(-0.4,1.4456832294801,16.));
#11587=CARTESIAN_POINT('Origin',(0.,0.,15.));
#11588=CARTESIAN_POINT('Origin',(0.,0.,2.));
#11589=CARTESIAN_POINT('',(2.,1.5,2.));
#11590=CARTESIAN_POINT('',(-2.,1.5,2.));
#11591=CARTESIAN_POINT('Origin',(0.,0.,2.));
#11592=CARTESIAN_POINT('',(-2.,-1.5,2.));
#11593=CARTESIAN_POINT('',(-2.,1.5,2.));
#11594=CARTESIAN_POINT('',(2.,-1.5,2.));
#11595=CARTESIAN_POINT('Origin',(0.,0.,2.));
#11596=CARTESIAN_POINT('',(2.,1.5,2.));
#11597=CARTESIAN_POINT('Origin',(0.,0.,2.));
#11598=CARTESIAN_POINT('',(2.,1.5,0.));
#11599=CARTESIAN_POINT('',(-2.,1.5,0.));
#11600=CARTESIAN_POINT('Origin',(0.,0.,0.));
#11601=CARTESIAN_POINT('',(-2.,1.5,2.));
#11602=CARTESIAN_POINT('',(2.,1.5,2.));
#11603=CARTESIAN_POINT('Origin',(-2.,1.5,2.));
#11604=CARTESIAN_POINT('',(-2.,-1.5,0.));
#11605=CARTESIAN_POINT('',(-2.,1.5,0.));
#11606=CARTESIAN_POINT('',(-2.,-1.5,2.));
#11607=CARTESIAN_POINT('Origin',(0.,0.,2.));
#11608=CARTESIAN_POINT('',(2.,-1.5,0.));
#11609=CARTESIAN_POINT('Origin',(0.,0.,0.));
#11610=CARTESIAN_POINT('',(2.,-1.5,2.));
#11611=CARTESIAN_POINT('Origin',(2.,1.5,2.));
#11612=CARTESIAN_POINT('',(2.,1.5,0.));
#11613=CARTESIAN_POINT('Origin',(0.,0.,0.));
#11614=CARTESIAN_POINT('Origin',(0.,0.,16.));
#11615=CARTESIAN_POINT('',(-1.4456832294801,-0.4,16.));
#11616=CARTESIAN_POINT('',(0.4,1.4456832294801,16.));
#11617=CARTESIAN_POINT('Origin',(0.,0.,16.));
#11618=CARTESIAN_POINT('',(-1.1842719282327,-0.4,16.));
#11619=CARTESIAN_POINT('',(0.4,1.1842719282327,16.));
#11620=CARTESIAN_POINT('Origin',(0.,0.,17.));
#11621=CARTESIAN_POINT('',(-1.4456832294801,-0.4,17.));
#11622=CARTESIAN_POINT('',(0.4,1.4456832294801,17.));
#11623=CARTESIAN_POINT('Origin',(0.,0.,17.));
#11624=CARTESIAN_POINT('',(-1.4456832294801,-0.4,16.));
#11625=CARTESIAN_POINT('',(0.4,1.4456832294801,16.));
#11626=CARTESIAN_POINT('Origin',(0.,0.,17.));
#11627=CARTESIAN_POINT('',(-1.1842719282327,0.4,17.));
#11628=CARTESIAN_POINT('',(-1.1842719282327,-0.4,17.));
#11629=CARTESIAN_POINT('',(0.4,1.1842719282327,17.));
#11630=CARTESIAN_POINT('',(-0.4,1.1842719282327,17.));
#11631=CARTESIAN_POINT('Origin',(0.4,1.1842719282327,16.));
#11632=CARTESIAN_POINT('Origin',(-0.4,1.1842719282327,16.));
#11633=CARTESIAN_POINT('Origin',(-1.1842719282327,0.4,16.));
#11634=CARTESIAN_POINT('Origin',(-1.1842719282327,-0.4,16.));
#11635=CARTESIAN_POINT('',(0.,0.,0.));
#11636=CARTESIAN_POINT('Origin',(31.,3.5,0.5));
#11637=CARTESIAN_POINT('',(29.197224362268,0.5,0.5));
#11638=CARTESIAN_POINT('',(29.197224362268,6.5,0.5));
#11639=CARTESIAN_POINT('Origin',(31.,3.5,0.5));
#11640=CARTESIAN_POINT('',(29.197224362268,6.5,0.));
#11641=CARTESIAN_POINT('',(29.197224362268,6.5,0.5));
#11642=CARTESIAN_POINT('',(29.197224362268,0.5,0.));
#11643=CARTESIAN_POINT('Origin',(31.,3.5,0.));
#11644=CARTESIAN_POINT('',(29.197224362268,0.5,0.5));
#11645=CARTESIAN_POINT('Origin',(0.,3.5,2.5));
#11646=CARTESIAN_POINT('',(1.80277563773199,6.5,2.5));
#11647=CARTESIAN_POINT('',(1.802775637732,0.500000000000001,2.5));
#11648=CARTESIAN_POINT('Origin',(0.,3.5,2.5));
#11649=CARTESIAN_POINT('',(1.80277563773199,6.5,3.));
#11650=CARTESIAN_POINT('',(1.80277563773199,6.5,2.5));
#11651=CARTESIAN_POINT('',(1.802775637732,0.500000000000001,3.));
#11652=CARTESIAN_POINT('Origin',(0.,3.5,3.));
#11653=CARTESIAN_POINT('',(1.802775637732,0.500000000000001,2.5));
#11654=CARTESIAN_POINT('Origin',(31.,3.5,3.));
#11655=CARTESIAN_POINT('',(32.5,3.5,3.));
#11656=CARTESIAN_POINT('Origin',(31.,3.5,3.));
#11657=CARTESIAN_POINT('',(32.5,3.5,0.));
#11658=CARTESIAN_POINT('',(32.5,3.5,3.));
#11659=CARTESIAN_POINT('Origin',(31.,3.5,0.));
#11660=CARTESIAN_POINT('Origin',(0.,3.5,3.));
#11661=CARTESIAN_POINT('',(1.5,3.5,3.));
#11662=CARTESIAN_POINT('Origin',(0.,3.5,3.));
#11663=CARTESIAN_POINT('',(1.5,3.5,0.));
#11664=CARTESIAN_POINT('',(1.5,3.5,3.));
#11665=CARTESIAN_POINT('Origin',(0.,3.5,0.));
#11666=CARTESIAN_POINT('Origin',(0.,3.5,3.));
#11667=CARTESIAN_POINT('',(0.,7.,3.));
#11668=CARTESIAN_POINT('',(0.,0.,3.));
#11669=CARTESIAN_POINT('Origin',(0.,3.5,3.));
#11670=CARTESIAN_POINT('',(0.,7.,0.));
#11671=CARTESIAN_POINT('',(0.,7.,3.));
#11672=CARTESIAN_POINT('',(0.,0.,0.));
#11673=CARTESIAN_POINT('Origin',(0.,3.5,0.));
#11674=CARTESIAN_POINT('',(0.,0.,3.));
#11675=CARTESIAN_POINT('Origin',(0.,0.,0.));
#11676=CARTESIAN_POINT('',(31.,7.,0.));
#11677=CARTESIAN_POINT('',(0.,7.,0.));
#11678=CARTESIAN_POINT('',(31.,0.,0.));
#11679=CARTESIAN_POINT('Origin',(31.,3.5,0.));
#11680=CARTESIAN_POINT('',(0.,0.,0.));
#11681=CARTESIAN_POINT('',(1.80277563773199,6.5,0.));
#11682=CARTESIAN_POINT('',(1.802775637732,0.500000000000001,0.));
#11683=CARTESIAN_POINT('Origin',(0.,3.5,0.));
#11684=CARTESIAN_POINT('',(1.802775637732,0.500000000000001,0.));
#11685=CARTESIAN_POINT('',(1.80277563773199,6.5,0.));
#11686=CARTESIAN_POINT('Origin',(0.,7.,3.));
#11687=CARTESIAN_POINT('',(31.,7.,3.));
#11688=CARTESIAN_POINT('',(0.,7.,3.));
#11689=CARTESIAN_POINT('',(31.,7.,3.));
#11690=CARTESIAN_POINT('Origin',(0.,0.,3.));
#11691=CARTESIAN_POINT('',(31.,0.,3.));
#11692=CARTESIAN_POINT('',(31.,0.,3.));
#11693=CARTESIAN_POINT('',(0.,0.,3.));
#11694=CARTESIAN_POINT('Origin',(31.,3.5,3.));
#11695=CARTESIAN_POINT('Origin',(31.,3.5,3.));
#11696=CARTESIAN_POINT('Origin',(0.,0.,3.));
#11697=CARTESIAN_POINT('',(29.197224362268,6.5,3.));
#11698=CARTESIAN_POINT('',(1.80277563773199,6.5,3.));
#11699=CARTESIAN_POINT('',(29.197224362268,0.5,3.));
#11700=CARTESIAN_POINT('Origin',(31.,3.5,3.));
#11701=CARTESIAN_POINT('',(1.802775637732,0.500000000000001,3.));
#11702=CARTESIAN_POINT('Origin',(1.80277563773199,6.5,2.5));
#11703=CARTESIAN_POINT('',(29.197224362268,6.5,2.5));
#11704=CARTESIAN_POINT('',(1.80277563773199,6.5,2.5));
#11705=CARTESIAN_POINT('',(29.197224362268,6.5,2.5));
#11706=CARTESIAN_POINT('Origin',(31.,3.5,2.5));
#11707=CARTESIAN_POINT('',(29.197224362268,0.5,2.5));
#11708=CARTESIAN_POINT('Origin',(31.,3.5,2.5));
#11709=CARTESIAN_POINT('',(29.197224362268,0.5,2.5));
#11710=CARTESIAN_POINT('Origin',(1.802775637732,0.500000000000001,2.5));
#11711=CARTESIAN_POINT('',(1.802775637732,0.500000000000001,2.5));
#11712=CARTESIAN_POINT('Origin',(0.,3.5,2.5));
#11713=CARTESIAN_POINT('Origin',(0.,3.5,0.5));
#11714=CARTESIAN_POINT('',(1.80277563773199,6.5,0.5));
#11715=CARTESIAN_POINT('',(1.80277563773199,6.5,0.5));
#11716=CARTESIAN_POINT('',(1.802775637732,0.500000000000001,0.5));
#11717=CARTESIAN_POINT('Origin',(0.,3.5,0.5));
#11718=CARTESIAN_POINT('',(1.802775637732,0.500000000000001,0.5));
#11719=CARTESIAN_POINT('Origin',(1.802775637732,0.500000000000001,0.5));
#11720=CARTESIAN_POINT('',(1.802775637732,0.500000000000001,0.5));
#11721=CARTESIAN_POINT('Origin',(1.80277563773199,6.5,0.5));
#11722=CARTESIAN_POINT('',(1.80277563773199,6.5,0.5));
#11723=CARTESIAN_POINT('Origin',(0.,3.5,0.5));
#11724=CARTESIAN_POINT('',(0.,0.,0.));
#11725=CARTESIAN_POINT('Origin',(0.,0.,16.));
#11726=CARTESIAN_POINT('',(1.25,-1.53080849893419E-16,15.));
#11727=CARTESIAN_POINT('Origin',(0.,0.,15.));
#11728=CARTESIAN_POINT('',(1.25,-1.53080849893419E-16,16.));
#11729=CARTESIAN_POINT('',(1.25,-1.53080849893419E-16,16.));
#11730=CARTESIAN_POINT('',(-1.1842719282327,-0.4,16.));
#11731=CARTESIAN_POINT('Origin',(0.,0.,16.));
#11732=CARTESIAN_POINT('',(-1.1842719282327,-0.4,17.));
#11733=CARTESIAN_POINT('',(-1.1842719282327,-0.4,16.));
#11734=CARTESIAN_POINT('',(-1.1842719282327,0.4,17.));
#11735=CARTESIAN_POINT('Origin',(0.,0.,17.));
#11736=CARTESIAN_POINT('',(-1.1842719282327,0.4,16.));
#11737=CARTESIAN_POINT('',(-1.1842719282327,0.4,16.));
#11738=CARTESIAN_POINT('',(-0.4,1.1842719282327,16.));
#11739=CARTESIAN_POINT('Origin',(0.,0.,16.));
#11740=CARTESIAN_POINT('',(-0.4,1.1842719282327,17.));
#11741=CARTESIAN_POINT('',(-0.4,1.1842719282327,16.));
#11742=CARTESIAN_POINT('',(0.4,1.1842719282327,17.));
#11743=CARTESIAN_POINT('Origin',(0.,0.,17.));
#11744=CARTESIAN_POINT('',(0.4,1.1842719282327,16.));
#11745=CARTESIAN_POINT('',(0.4,1.1842719282327,16.));
#11746=CARTESIAN_POINT('Origin',(0.,0.,16.));
#11747=CARTESIAN_POINT('Origin',(0.,0.,15.));
#11748=CARTESIAN_POINT('',(1.5,-1.83697019872103E-16,4.));
#11749=CARTESIAN_POINT('Origin',(0.,0.,4.));
#11750=CARTESIAN_POINT('',(1.5,-1.83697019872103E-16,15.));
#11751=CARTESIAN_POINT('',(1.5,-1.83697019872103E-16,15.));
#11752=CARTESIAN_POINT('Origin',(0.,0.,15.));
#11753=CARTESIAN_POINT('Origin',(0.,0.,16.));
#11754=CARTESIAN_POINT('',(-1.4456832294801,0.4,16.));
#11755=CARTESIAN_POINT('',(-1.1842719282327,0.4,16.));
#11756=CARTESIAN_POINT('',(-0.4,1.4456832294801,16.));
#11757=CARTESIAN_POINT('Origin',(0.,0.,16.));
#11758=CARTESIAN_POINT('',(-0.4,1.1842719282327,16.));
#11759=CARTESIAN_POINT('Origin',(0.,0.,17.));
#11760=CARTESIAN_POINT('',(-1.4456832294801,0.4,17.));
#11761=CARTESIAN_POINT('',(-1.4456832294801,0.4,16.));
#11762=CARTESIAN_POINT('',(-0.4,1.4456832294801,17.));
#11763=CARTESIAN_POINT('Origin',(0.,0.,17.));
#11764=CARTESIAN_POINT('',(-0.4,1.4456832294801,16.));
#11765=CARTESIAN_POINT('Origin',(0.,0.,15.));
#11766=CARTESIAN_POINT('Origin',(0.,0.,16.));
#11767=CARTESIAN_POINT('',(-1.4456832294801,-0.4,16.));
#11768=CARTESIAN_POINT('',(0.4,1.4456832294801,16.));
#11769=CARTESIAN_POINT('Origin',(0.,0.,16.));
#11770=CARTESIAN_POINT('',(-1.1842719282327,-0.4,16.));
#11771=CARTESIAN_POINT('',(0.4,1.1842719282327,16.));
#11772=CARTESIAN_POINT('Origin',(0.,0.,17.));
#11773=CARTESIAN_POINT('',(-1.4456832294801,-0.4,17.));
#11774=CARTESIAN_POINT('',(0.4,1.4456832294801,17.));
#11775=CARTESIAN_POINT('Origin',(0.,0.,17.));
#11776=CARTESIAN_POINT('',(-1.4456832294801,-0.4,16.));
#11777=CARTESIAN_POINT('',(0.4,1.4456832294801,16.));
#11778=CARTESIAN_POINT('Origin',(0.,0.,17.));
#11779=CARTESIAN_POINT('',(-1.1842719282327,0.4,17.));
#11780=CARTESIAN_POINT('',(-1.1842719282327,-0.4,17.));
#11781=CARTESIAN_POINT('',(0.4,1.1842719282327,17.));
#11782=CARTESIAN_POINT('',(-0.4,1.1842719282327,17.));
#11783=CARTESIAN_POINT('Origin',(0.4,1.1842719282327,16.));
#11784=CARTESIAN_POINT('Origin',(-0.4,1.1842719282327,16.));
#11785=CARTESIAN_POINT('Origin',(-1.1842719282327,0.4,16.));
#11786=CARTESIAN_POINT('Origin',(-1.1842719282327,-0.4,16.));
#11787=CARTESIAN_POINT('Origin',(0.,0.,4.));
#11788=CARTESIAN_POINT('',(-2.,1.5,4.));
#11789=CARTESIAN_POINT('',(2.,1.5,4.));
#11790=CARTESIAN_POINT('Origin',(0.,0.,4.));
#11791=CARTESIAN_POINT('',(-2.,-1.5,4.));
#11792=CARTESIAN_POINT('',(-2.,1.5,4.));
#11793=CARTESIAN_POINT('',(2.,-1.5,4.));
#11794=CARTESIAN_POINT('Origin',(0.,0.,4.));
#11795=CARTESIAN_POINT('',(2.,1.5,4.));
#11796=CARTESIAN_POINT('Origin',(0.,0.,2.));
#11797=CARTESIAN_POINT('',(2.,1.5,2.));
#11798=CARTESIAN_POINT('',(2.,1.5,2.));
#11799=CARTESIAN_POINT('',(-2.,1.5,2.));
#11800=CARTESIAN_POINT('Origin',(0.,0.,2.));
#11801=CARTESIAN_POINT('',(-2.,1.5,2.));
#11802=CARTESIAN_POINT('Origin',(2.,1.5,2.));
#11803=CARTESIAN_POINT('',(2.,-1.5,2.));
#11804=CARTESIAN_POINT('',(2.,-1.5,2.));
#11805=CARTESIAN_POINT('',(2.,1.5,2.));
#11806=CARTESIAN_POINT('Origin',(0.,0.,2.));
#11807=CARTESIAN_POINT('',(-2.,-1.5,2.));
#11808=CARTESIAN_POINT('',(-2.,-1.5,2.));
#11809=CARTESIAN_POINT('Origin',(0.,0.,2.));
#11810=CARTESIAN_POINT('Origin',(-2.,1.5,2.));
#11811=CARTESIAN_POINT('',(-2.,1.5,2.));
#11812=CARTESIAN_POINT('Origin',(0.,0.,2.));
#11813=CARTESIAN_POINT('',(0.,0.,0.));
#11814=CARTESIAN_POINT('Origin',(0.,0.,-1.9));
#11815=CARTESIAN_POINT('',(2.5,3.06161699786838E-16,-1.9));
#11816=CARTESIAN_POINT('',(-2.5,-3.06161699786838E-16,-1.9));
#11817=CARTESIAN_POINT('Origin',(0.,0.,-1.9));
#11818=CARTESIAN_POINT('Origin',(0.,0.,-1.9));
#11819=CARTESIAN_POINT('',(-2.4,-2.93915231795365E-16,-2.));
#11820=CARTESIAN_POINT('Origin',(-2.4,-2.93915231795365E-16,-1.9));
#11821=CARTESIAN_POINT('Origin',(0.,0.,-2.));
#11822=CARTESIAN_POINT('Origin',(0.,0.,1.));
#11823=CARTESIAN_POINT('',(-1.1842719282327,0.4,1.));
#11824=CARTESIAN_POINT('',(-1.1842719282327,-0.4,1.));
#11825=CARTESIAN_POINT('Origin',(0.,0.,1.));
#11826=CARTESIAN_POINT('',(-1.1842719282327,-0.4,0.));
#11827=CARTESIAN_POINT('',(-1.1842719282327,-0.4,1.));
#11828=CARTESIAN_POINT('',(-1.1842719282327,0.4,0.));
#11829=CARTESIAN_POINT('Origin',(0.,0.,0.));
#11830=CARTESIAN_POINT('',(-1.1842719282327,0.4,1.));
#11831=CARTESIAN_POINT('Origin',(0.,0.,1.));
#11832=CARTESIAN_POINT('',(2.5,-3.06161699786838E-16,1.));
#11833=CARTESIAN_POINT('',(2.5,-3.06161699786838E-16,1.));
#11834=CARTESIAN_POINT('Origin',(0.,0.,1.));
#11835=CARTESIAN_POINT('Origin',(0.,0.,1.));
#11836=CARTESIAN_POINT('',(-1.4456832294801,0.4,0.));
#11837=CARTESIAN_POINT('',(-1.4456832294801,-0.4,0.));
#11838=CARTESIAN_POINT('Origin',(0.,0.,0.));
#11839=CARTESIAN_POINT('',(-1.4456832294801,-0.4,1.));
#11840=CARTESIAN_POINT('',(-1.4456832294801,-0.4,1.));
#11841=CARTESIAN_POINT('',(1.5,-1.83697019872103E-16,1.));
#11842=CARTESIAN_POINT('Origin',(0.,0.,1.));
#11843=CARTESIAN_POINT('',(1.5,-1.83697019872103E-16,-1.));
#11844=CARTESIAN_POINT('',(1.5,-1.83697019872103E-16,1.));
#11845=CARTESIAN_POINT('Origin',(0.,0.,-1.));
#11846=CARTESIAN_POINT('',(0.4,1.4456832294801,1.));
#11847=CARTESIAN_POINT('Origin',(0.,0.,1.));
#11848=CARTESIAN_POINT('',(0.4,1.4456832294801,0.));
#11849=CARTESIAN_POINT('',(0.4,1.4456832294801,1.));
#11850=CARTESIAN_POINT('',(-0.4,1.4456832294801,0.));
#11851=CARTESIAN_POINT('Origin',(0.,0.,0.));
#11852=CARTESIAN_POINT('',(-0.4,1.4456832294801,1.));
#11853=CARTESIAN_POINT('',(-0.4,1.4456832294801,1.));
#11854=CARTESIAN_POINT('',(-1.4456832294801,0.4,1.));
#11855=CARTESIAN_POINT('Origin',(0.,0.,1.));
#11856=CARTESIAN_POINT('',(-1.4456832294801,0.4,1.));
#11857=CARTESIAN_POINT('Origin',(0.,0.,0.));
#11858=CARTESIAN_POINT('',(0.4,1.1842719282327,0.));
#11859=CARTESIAN_POINT('',(0.4,1.1842719282327,0.));
#11860=CARTESIAN_POINT('',(-0.4,1.1842719282327,0.));
#11861=CARTESIAN_POINT('Origin',(0.,0.,0.));
#11862=CARTESIAN_POINT('',(-0.4,1.1842719282327,0.));
#11863=CARTESIAN_POINT('Origin',(0.,0.,0.));
#11864=CARTESIAN_POINT('',(-1.1842719282327,0.4,0.));
#11865=CARTESIAN_POINT('',(-1.1842719282327,-0.4,0.));
#11866=CARTESIAN_POINT('Origin',(0.,0.,1.));
#11867=CARTESIAN_POINT('',(-0.4,1.1842719282327,1.));
#11868=CARTESIAN_POINT('',(-0.4,1.1842719282327,1.));
#11869=CARTESIAN_POINT('',(0.4,1.1842719282327,1.));
#11870=CARTESIAN_POINT('Origin',(0.,0.,1.));
#11871=CARTESIAN_POINT('',(0.4,1.1842719282327,1.));
#11872=CARTESIAN_POINT('',(-1.1842719282327,-0.4,1.));
#11873=CARTESIAN_POINT('',(-1.1842719282327,0.4,1.));
#11874=CARTESIAN_POINT('Origin',(0.,0.,1.));
#11875=CARTESIAN_POINT('',(0.4,1.1842719282327,1.));
#11876=CARTESIAN_POINT('',(-0.4,1.1842719282327,1.));
#11877=CARTESIAN_POINT('Origin',(-0.4,1.1842719282327,1.));
#11878=CARTESIAN_POINT('Origin',(-1.1842719282327,0.4,1.));
#11879=CARTESIAN_POINT('Origin',(-1.1842719282327,-0.4,1.));
#11880=CARTESIAN_POINT('Origin',(0.4,1.1842719282327,1.));
#11881=CARTESIAN_POINT('Origin',(0.,0.,-2.));
#11882=CARTESIAN_POINT('Origin',(0.,0.,-1.));
#11883=CARTESIAN_POINT('',(5.37382075471697,5.20193281178138,59.5));
#11884=CARTESIAN_POINT('',(18.873820754717,5.20193281178138,52.5));
#11885=CARTESIAN_POINT('',(-8.12617924528225,5.2019328117826,54.5));
#11886=CARTESIAN_POINT('',(18.8738207547162,5.20193281178421,54.5));
#11887=CARTESIAN_POINT('',(18.8428797401373,5.12716423978079,58.5));
#11888=CARTESIAN_POINT('',(22.107844593972,3.86361677768567,64.5));
#11889=CARTESIAN_POINT('',(18.873820754717,5.20193281178138,68.5));
#11890=CARTESIAN_POINT('',(30.7274770567354,33.8461439594749,63.5));
#11891=CARTESIAN_POINT('',(10.6238207547164,25.6019328117816,52.5));
#11892=CARTESIAN_POINT('',(-8.12617924528304,5.20193281178138,52.5));
#11893=CARTESIAN_POINT('',(-8.10325220752136,5.12433102905749,58.5));
#11894=CARTESIAN_POINT('',(-20.2662121707959,33.9398798603704,64.5));
#11895=CARTESIAN_POINT('',(-8.12617924528305,5.20193281178139,68.5));
#11896=CARTESIAN_POINT('',(-16.9096412402919,34.9315610533576,60.5));
#11897=CARTESIAN_POINT('',(-16.9096412403003,34.9315610533536,52.5));
#11898=CARTESIAN_POINT('',(30.7274770567364,33.8461439594739,52.5));
#11899=CARTESIAN_POINT('',(30.7274770567364,33.8461439594739,68.5));
#11900=CARTESIAN_POINT('',(-16.9096412403003,34.9315610533536,68.5));
#11901=CARTESIAN_POINT('',(3.48013161337589,26.5944938527695,56.5));
#11902=CARTESIAN_POINT('',(-12.0237450383966,54.3366965188633,64.5));
#11903=CARTESIAN_POINT('',(13.8575330742423,24.2628642420256,64.5));
#11904=CARTESIAN_POINT('',(13.8575330742422,24.2628642420256,56.5));
#11905=CARTESIAN_POINT('',(22.4841423725807,54.2433847847668,52.5));
#11906=CARTESIAN_POINT('',(-8.6674341797561,55.3292575598495,52.5));
#11907=CARTESIAN_POINT('',(0.123820754716976,25.6019328117814,52.5));
#11908=CARTESIAN_POINT('',(0.123820754716973,25.6019328117814,68.5));
#11909=CARTESIAN_POINT('',(22.4841423725807,54.2433847847668,68.5));
#11910=CARTESIAN_POINT('',(10.623820754717,25.6019328117814,68.5));
#11911=CARTESIAN_POINT('',(-8.6674341797561,55.3292575598495,68.5));
#11912=UNCERTAINTY_MEASURE_WITH_UNIT(LENGTH_MEASURE(0.01),#11934,
'DISTANCE_ACCURACY_VALUE',
'Maximum model space distance between geometric entities at asserted c
onnectivities');
#11913=UNCERTAINTY_MEASURE_WITH_UNIT(LENGTH_MEASURE(0.01),#11934,
'DISTANCE_ACCURACY_VALUE',
'Maximum model space distance between geometric entities at asserted c
onnectivities');
#11914=UNCERTAINTY_MEASURE_WITH_UNIT(LENGTH_MEASURE(0.01),#11934,
'DISTANCE_ACCURACY_VALUE',
'Maximum model space distance between geometric entities at asserted c
onnectivities');
#11915=UNCERTAINTY_MEASURE_WITH_UNIT(LENGTH_MEASURE(0.01),#11934,
'DISTANCE_ACCURACY_VALUE',
'Maximum model space distance between geometric entities at asserted c
onnectivities');
#11916=UNCERTAINTY_MEASURE_WITH_UNIT(LENGTH_MEASURE(0.01),#11934,
'DISTANCE_ACCURACY_VALUE',
'Maximum model space distance between geometric entities at asserted c
onnectivities');
#11917=UNCERTAINTY_MEASURE_WITH_UNIT(LENGTH_MEASURE(0.01),#11934,
'DISTANCE_ACCURACY_VALUE',
'Maximum model space distance between geometric entities at asserted c
onnectivities');
#11918=UNCERTAINTY_MEASURE_WITH_UNIT(LENGTH_MEASURE(0.01),#11934,
'DISTANCE_ACCURACY_VALUE',
'Maximum model space distance between geometric entities at asserted c
onnectivities');
#11919=UNCERTAINTY_MEASURE_WITH_UNIT(LENGTH_MEASURE(0.01),#11934,
'DISTANCE_ACCURACY_VALUE',
'Maximum model space distance between geometric entities at asserted c
onnectivities');
#11920=UNCERTAINTY_MEASURE_WITH_UNIT(LENGTH_MEASURE(0.01),#11934,
'DISTANCE_ACCURACY_VALUE',
'Maximum model space distance between geometric entities at asserted c
onnectivities');
#11921=UNCERTAINTY_MEASURE_WITH_UNIT(LENGTH_MEASURE(0.01),#11934,
'DISTANCE_ACCURACY_VALUE',
'Maximum model space distance between geometric entities at asserted c
onnectivities');
#11922=UNCERTAINTY_MEASURE_WITH_UNIT(LENGTH_MEASURE(0.01),#11934,
'DISTANCE_ACCURACY_VALUE',
'Maximum model space distance between geometric entities at asserted c
onnectivities');
#11923=(
GEOMETRIC_REPRESENTATION_CONTEXT(3)
GLOBAL_UNCERTAINTY_ASSIGNED_CONTEXT((#11912))
GLOBAL_UNIT_ASSIGNED_CONTEXT((#11934,#11936,#11937))
REPRESENTATION_CONTEXT('','3D')
);
#11924=(
GEOMETRIC_REPRESENTATION_CONTEXT(3)
GLOBAL_UNCERTAINTY_ASSIGNED_CONTEXT((#11913))
GLOBAL_UNIT_ASSIGNED_CONTEXT((#11934,#11936,#11937))
REPRESENTATION_CONTEXT('','3D')
);
#11925=(
GEOMETRIC_REPRESENTATION_CONTEXT(3)
GLOBAL_UNCERTAINTY_ASSIGNED_CONTEXT((#11914))
GLOBAL_UNIT_ASSIGNED_CONTEXT((#11934,#11936,#11937))
REPRESENTATION_CONTEXT('','3D')
);
#11926=(
GEOMETRIC_REPRESENTATION_CONTEXT(3)
GLOBAL_UNCERTAINTY_ASSIGNED_CONTEXT((#11915))
GLOBAL_UNIT_ASSIGNED_CONTEXT((#11934,#11936,#11937))
REPRESENTATION_CONTEXT('','3D')
);
#11927=(
GEOMETRIC_REPRESENTATION_CONTEXT(3)
GLOBAL_UNCERTAINTY_ASSIGNED_CONTEXT((#11916))
GLOBAL_UNIT_ASSIGNED_CONTEXT((#11934,#11936,#11937))
REPRESENTATION_CONTEXT('','3D')
);
#11928=(
GEOMETRIC_REPRESENTATION_CONTEXT(3)
GLOBAL_UNCERTAINTY_ASSIGNED_CONTEXT((#11917))
GLOBAL_UNIT_ASSIGNED_CONTEXT((#11934,#11936,#11937))
REPRESENTATION_CONTEXT('','3D')
);
#11929=(
GEOMETRIC_REPRESENTATION_CONTEXT(3)
GLOBAL_UNCERTAINTY_ASSIGNED_CONTEXT((#11918))
GLOBAL_UNIT_ASSIGNED_CONTEXT((#11934,#11936,#11937))
REPRESENTATION_CONTEXT('','3D')
);
#11930=(
GEOMETRIC_REPRESENTATION_CONTEXT(3)
GLOBAL_UNCERTAINTY_ASSIGNED_CONTEXT((#11919))
GLOBAL_UNIT_ASSIGNED_CONTEXT((#11934,#11936,#11937))
REPRESENTATION_CONTEXT('','3D')
);
#11931=(
GEOMETRIC_REPRESENTATION_CONTEXT(3)
GLOBAL_UNCERTAINTY_ASSIGNED_CONTEXT((#11920))
GLOBAL_UNIT_ASSIGNED_CONTEXT((#11934,#11936,#11937))
REPRESENTATION_CONTEXT('','3D')
);
#11932=(
GEOMETRIC_REPRESENTATION_CONTEXT(3)
GLOBAL_UNCERTAINTY_ASSIGNED_CONTEXT((#11921))
GLOBAL_UNIT_ASSIGNED_CONTEXT((#11934,#11936,#11937))
REPRESENTATION_CONTEXT('','3D')
);
#11933=(
GEOMETRIC_REPRESENTATION_CONTEXT(3)
GLOBAL_UNCERTAINTY_ASSIGNED_CONTEXT((#11922))
GLOBAL_UNIT_ASSIGNED_CONTEXT((#11934,#11936,#11937))
REPRESENTATION_CONTEXT('','3D')
);
#11934=(
LENGTH_UNIT()
NAMED_UNIT(*)
SI_UNIT(.MILLI.,.METRE.)
);
#11935=(
LENGTH_UNIT()
NAMED_UNIT(*)
SI_UNIT($,.METRE.)
);
#11936=(
NAMED_UNIT(*)
PLANE_ANGLE_UNIT()
SI_UNIT($,.RADIAN.)
);
#11937=(
NAMED_UNIT(*)
SI_UNIT($,.STERADIAN.)
SOLID_ANGLE_UNIT()
);
#11938=SHAPE_DEFINITION_REPRESENTATION(#11948,#11987);
#11939=SHAPE_DEFINITION_REPRESENTATION(#11949,#11988);
#11940=SHAPE_DEFINITION_REPRESENTATION(#11950,#11989);
#11941=SHAPE_DEFINITION_REPRESENTATION(#11951,#11990);
#11942=SHAPE_DEFINITION_REPRESENTATION(#11952,#11991);
#11943=SHAPE_DEFINITION_REPRESENTATION(#11953,#11992);
#11944=SHAPE_DEFINITION_REPRESENTATION(#11954,#11993);
#11945=SHAPE_DEFINITION_REPRESENTATION(#11955,#11994);
#11946=SHAPE_DEFINITION_REPRESENTATION(#11956,#11995);
#11947=SHAPE_DEFINITION_REPRESENTATION(#11957,#11996);
#11948=PRODUCT_DEFINITION_SHAPE('',$,#11998);
#11949=PRODUCT_DEFINITION_SHAPE('',$,#11999);
#11950=PRODUCT_DEFINITION_SHAPE('',$,#12000);
#11951=PRODUCT_DEFINITION_SHAPE('',$,#12001);
#11952=PRODUCT_DEFINITION_SHAPE('',$,#12002);
#11953=PRODUCT_DEFINITION_SHAPE('',$,#12003);
#11954=PRODUCT_DEFINITION_SHAPE('',$,#12004);
#11955=PRODUCT_DEFINITION_SHAPE('',$,#12005);
#11956=PRODUCT_DEFINITION_SHAPE('',$,#12006);
#11957=PRODUCT_DEFINITION_SHAPE('',$,#12007);
#11958=PRODUCT_DEFINITION_SHAPE($,$,#98);
#11959=PRODUCT_DEFINITION_SHAPE($,$,#99);
#11960=PRODUCT_DEFINITION_SHAPE($,$,#100);
#11961=PRODUCT_DEFINITION_SHAPE($,$,#101);
#11962=PRODUCT_DEFINITION_SHAPE($,$,#102);
#11963=PRODUCT_DEFINITION_SHAPE($,$,#103);
#11964=PRODUCT_DEFINITION_SHAPE($,$,#104);
#11965=PRODUCT_DEFINITION_SHAPE($,$,#105);
#11966=PRODUCT_DEFINITION_SHAPE($,$,#106);
#11967=PRODUCT_DEFINITION_SHAPE($,$,#107);
#11968=PRODUCT_DEFINITION_SHAPE($,$,#108);
#11969=PRODUCT_DEFINITION_SHAPE($,$,#109);
#11970=PRODUCT_DEFINITION_SHAPE($,$,#110);
#11971=PRODUCT_DEFINITION_SHAPE($,$,#111);
#11972=PRODUCT_DEFINITION_SHAPE($,$,#112);
#11973=PRODUCT_DEFINITION_SHAPE($,$,#113);
#11974=PRODUCT_DEFINITION_SHAPE($,$,#114);
#11975=PRODUCT_DEFINITION_SHAPE($,$,#115);
#11976=PRODUCT_DEFINITION_SHAPE($,$,#116);
#11977=PRODUCT_DEFINITION_SHAPE($,$,#117);
#11978=PRODUCT_DEFINITION_SHAPE($,$,#118);
#11979=PRODUCT_DEFINITION_SHAPE($,$,#119);
#11980=PRODUCT_DEFINITION_SHAPE($,$,#120);
#11981=PRODUCT_DEFINITION_SHAPE($,$,#121);
#11982=PRODUCT_DEFINITION_SHAPE($,$,#122);
#11983=PRODUCT_DEFINITION_SHAPE($,$,#123);
#11984=PRODUCT_DEFINITION_SHAPE($,$,#124);
#11985=PRODUCT_DEFINITION_SHAPE($,$,#125);
#11986=PRODUCT_DEFINITION_SHAPE($,$,#126);
#11987=SHAPE_REPRESENTATION('',(#6752,#7621,#7622,#7623,#7624,#7625,#7626,
#7627,#7628,#7629,#7630,#7631,#7632,#7633,#7634,#7635,#7636,#7637,#7638,
#7639,#7640,#7641,#7642,#7643,#7644,#7645,#7646,#7647,#7648,#7649),#11923);
#11988=SHAPE_REPRESENTATION('',(#6753),#11924);
#11989=SHAPE_REPRESENTATION('',(#6800),#11925);
#11990=SHAPE_REPRESENTATION('',(#6849),#11926);
#11991=SHAPE_REPRESENTATION('',(#6899),#11927);
#11992=SHAPE_REPRESENTATION('',(#7448),#11928);
#11993=SHAPE_REPRESENTATION('',(#7486),#11929);
#11994=SHAPE_REPRESENTATION('',(#7521),#11930);
#11995=SHAPE_REPRESENTATION('',(#7556),#11931);
#11996=SHAPE_REPRESENTATION('',(#7591),#11932);
#11997=PRODUCT_DEFINITION_CONTEXT('part definition',#12029,'design');
#11998=PRODUCT_DEFINITION('MAT-009','MAT-009',#12008,#11997);
#11999=PRODUCT_DEFINITION('Mounting plate','Mounting Plate',#12009,#11997);
#12000=PRODUCT_DEFINITION('Short Drive Link','Short Drive Link',#12010,
#11997);
#12001=PRODUCT_DEFINITION('Long Drive Link','Long Drive Link',#12011,#11997);
#12002=PRODUCT_DEFINITION('Spur Gear','Spur Gear',#12012,#11997);
#12003=PRODUCT_DEFINITION('Gripper Jaw','Gripper Jaw',#12013,#11997);
#12004=PRODUCT_DEFINITION('Long Pivot Pin','Long Pivot Pin',#12014,#11997);
#12005=PRODUCT_DEFINITION('Linkage Arm','Linkage Arm',#12015,#11997);
#12006=PRODUCT_DEFINITION('Pivot pin','Pivot Pin',#12016,#11997);
#12007=PRODUCT_DEFINITION('Pin Cap','Pin Cap',#12017,#11997);
#12008=PRODUCT_DEFINITION_FORMATION('',$,#12031);
#12009=PRODUCT_DEFINITION_FORMATION('',$,#12032);
#12010=PRODUCT_DEFINITION_FORMATION('',$,#12033);
#12011=PRODUCT_DEFINITION_FORMATION('',$,#12034);
#12012=PRODUCT_DEFINITION_FORMATION('',$,#12035);
#12013=PRODUCT_DEFINITION_FORMATION('',$,#12036);
#12014=PRODUCT_DEFINITION_FORMATION('',$,#12037);
#12015=PRODUCT_DEFINITION_FORMATION('',$,#12038);
#12016=PRODUCT_DEFINITION_FORMATION('',$,#12039);
#12017=PRODUCT_DEFINITION_FORMATION('',$,#12040);
#12018=PRODUCT_RELATED_PRODUCT_CATEGORY('MAT-009','MAT-009',(#12031));
#12019=PRODUCT_RELATED_PRODUCT_CATEGORY('Mounting Plate',
'Mounting Plate',(#12032));
#12020=PRODUCT_RELATED_PRODUCT_CATEGORY('Short Drive Link',
'Short Drive Link',(#12033));
#12021=PRODUCT_RELATED_PRODUCT_CATEGORY('Long Drive Link',
'Long Drive Link',(#12034));
#12022=PRODUCT_RELATED_PRODUCT_CATEGORY('Spur Gear','Spur Gear',(#12035));
#12023=PRODUCT_RELATED_PRODUCT_CATEGORY('Gripper Jaw','Gripper Jaw',(#12036));
#12024=PRODUCT_RELATED_PRODUCT_CATEGORY('Long Pivot Pin',
'Long Pivot Pin',(#12037));
#12025=PRODUCT_RELATED_PRODUCT_CATEGORY('Linkage Arm','Linkage Arm',(#12038));
#12026=PRODUCT_RELATED_PRODUCT_CATEGORY('Pivot Pin','Pivot Pin',(#12039));
#12027=PRODUCT_RELATED_PRODUCT_CATEGORY('Pin Cap','Pin Cap',(#12040));
#12028=APPLICATION_PROTOCOL_DEFINITION('international standard',
'automotive_design',2009,#12029);
#12029=APPLICATION_CONTEXT(
'Core Data for Automotive Mechanical Design Process');
#12030=PRODUCT_CONTEXT('part definition',#12029,'mechanical');
#12031=PRODUCT('MAT-009','MAT-009','STEP AP214',(#12030));
#12032=PRODUCT('Mounting plate','Mounting Plate','Mounting plate',(#12030));
#12033=PRODUCT('Short Drive Link','Short Drive Link',$,(#12030));
#12034=PRODUCT('Long Drive Link','Long Drive Link',$,(#12030));
#12035=PRODUCT('Spur Gear','Spur Gear',$,(#12030));
#12036=PRODUCT('Gripper Jaw','Gripper Jaw',$,(#12030));
#12037=PRODUCT('Long Pivot Pin','Long Pivot Pin',$,(#12030));
#12038=PRODUCT('Linkage Arm','Linkage Arm',$,(#12030));
#12039=PRODUCT('Pivot pin','Pivot Pin','Pivot pin',(#12030));
#12040=PRODUCT('Pin Cap','Pin Cap',$,(#12030));
#12041=PRESENTATION_STYLE_ASSIGNMENT((#12045));
#12042=PRESENTATION_STYLE_ASSIGNMENT((#12046));
#12043=PRESENTATION_STYLE_ASSIGNMENT((#12047));
#12044=PRESENTATION_STYLE_ASSIGNMENT((#12048));
#12045=SURFACE_STYLE_USAGE(.BOTH.,#12049);
#12046=SURFACE_STYLE_USAGE(.BOTH.,#12050);
#12047=SURFACE_STYLE_USAGE(.BOTH.,#12051);
#12048=SURFACE_STYLE_USAGE(.BOTH.,#12052);
#12049=SURFACE_SIDE_STYLE('',(#12053));
#12050=SURFACE_SIDE_STYLE('',(#12054));
#12051=SURFACE_SIDE_STYLE('',(#12055));
#12052=SURFACE_SIDE_STYLE('',(#12056));
#12053=SURFACE_STYLE_FILL_AREA(#12057);
#12054=SURFACE_STYLE_FILL_AREA(#12058);
#12055=SURFACE_STYLE_FILL_AREA(#12059);
#12056=SURFACE_STYLE_FILL_AREA(#12060);
#12057=FILL_AREA_STYLE('Steel - Satin',(#12061));
#12058=FILL_AREA_STYLE('Opaque(227,224,212)',(#12062));
#12059=FILL_AREA_STYLE('Opaque(61,176,222)',(#12063));
#12060=FILL_AREA_STYLE('Opaque(97,158,199)',(#12064));
#12061=FILL_AREA_STYLE_COLOUR('Steel - Satin',#12065);
#12062=FILL_AREA_STYLE_COLOUR('Opaque(227,224,212)',#12066);
#12063=FILL_AREA_STYLE_COLOUR('Opaque(61,176,222)',#12067);
#12064=FILL_AREA_STYLE_COLOUR('Opaque(97,158,199)',#12068);
#12065=COLOUR_RGB('Steel - Satin',0.627450980392157,0.627450980392157,0.627450980392157);
#12066=COLOUR_RGB('Opaque(227,224,212)',0.890196078431372,0.87843137254902,
0.831372549019608);
#12067=COLOUR_RGB('Opaque(61,176,222)',0.23921568627451,0.690196078431373,
0.870588235294118);
#12068=COLOUR_RGB('Opaque(97,158,199)',0.380392156862745,0.619607843137255,
0.780392156862745);
ENDSEC;
END-ISO-10303-21;
